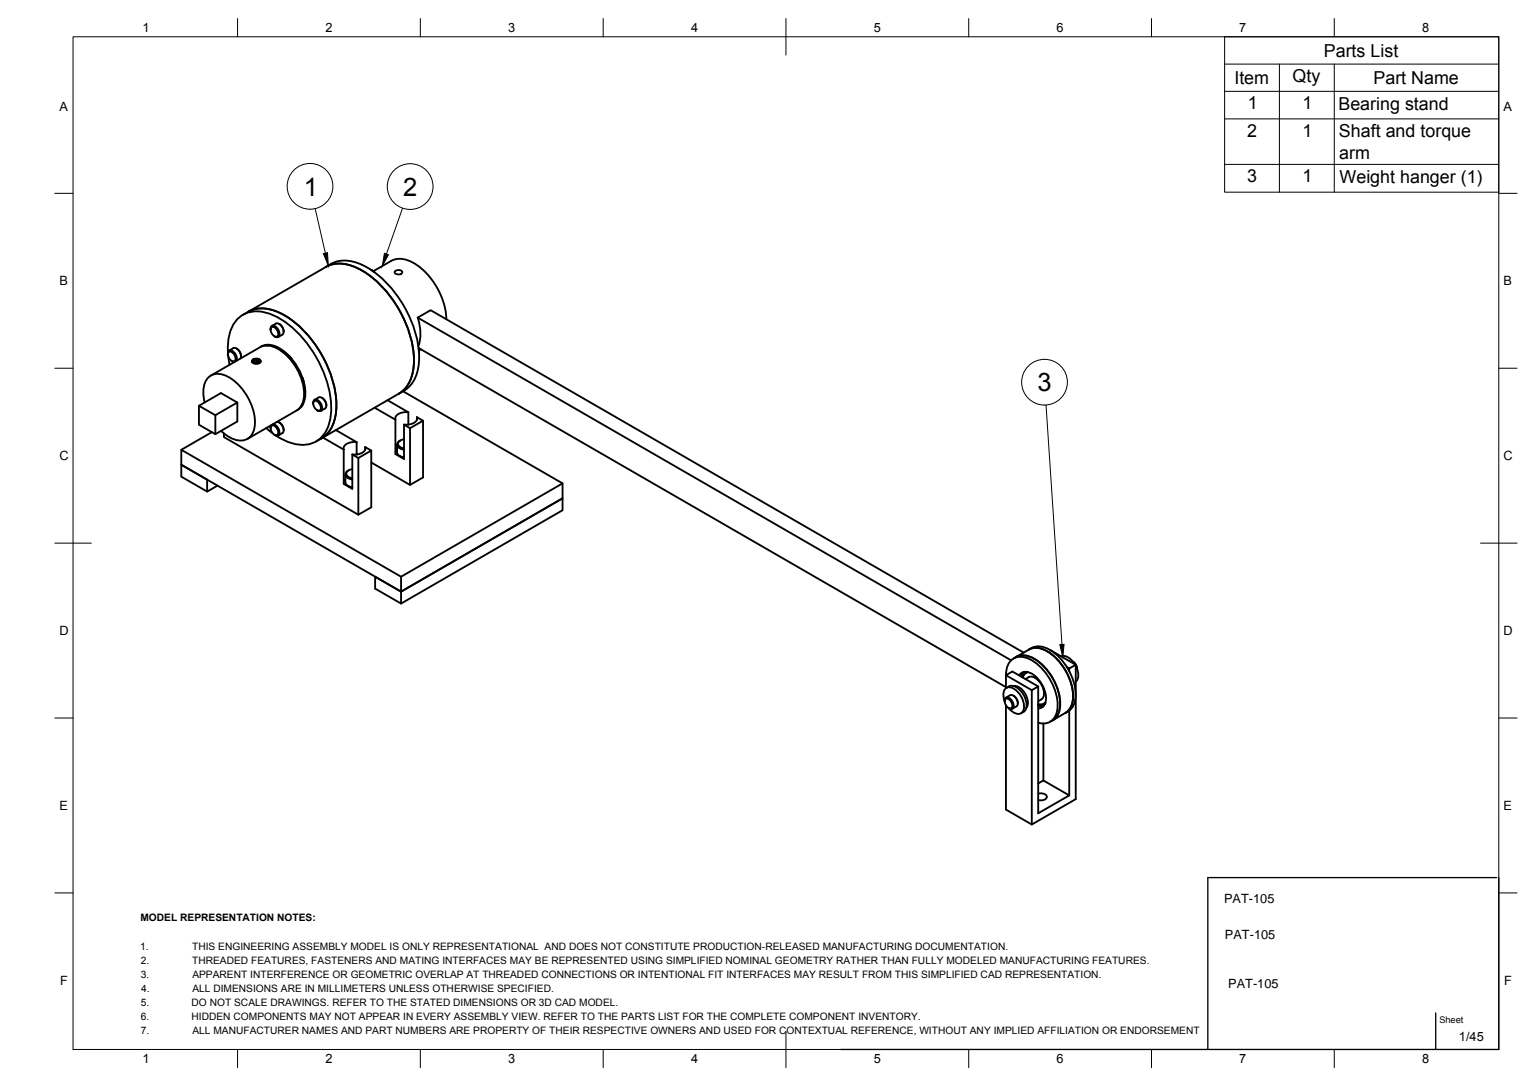
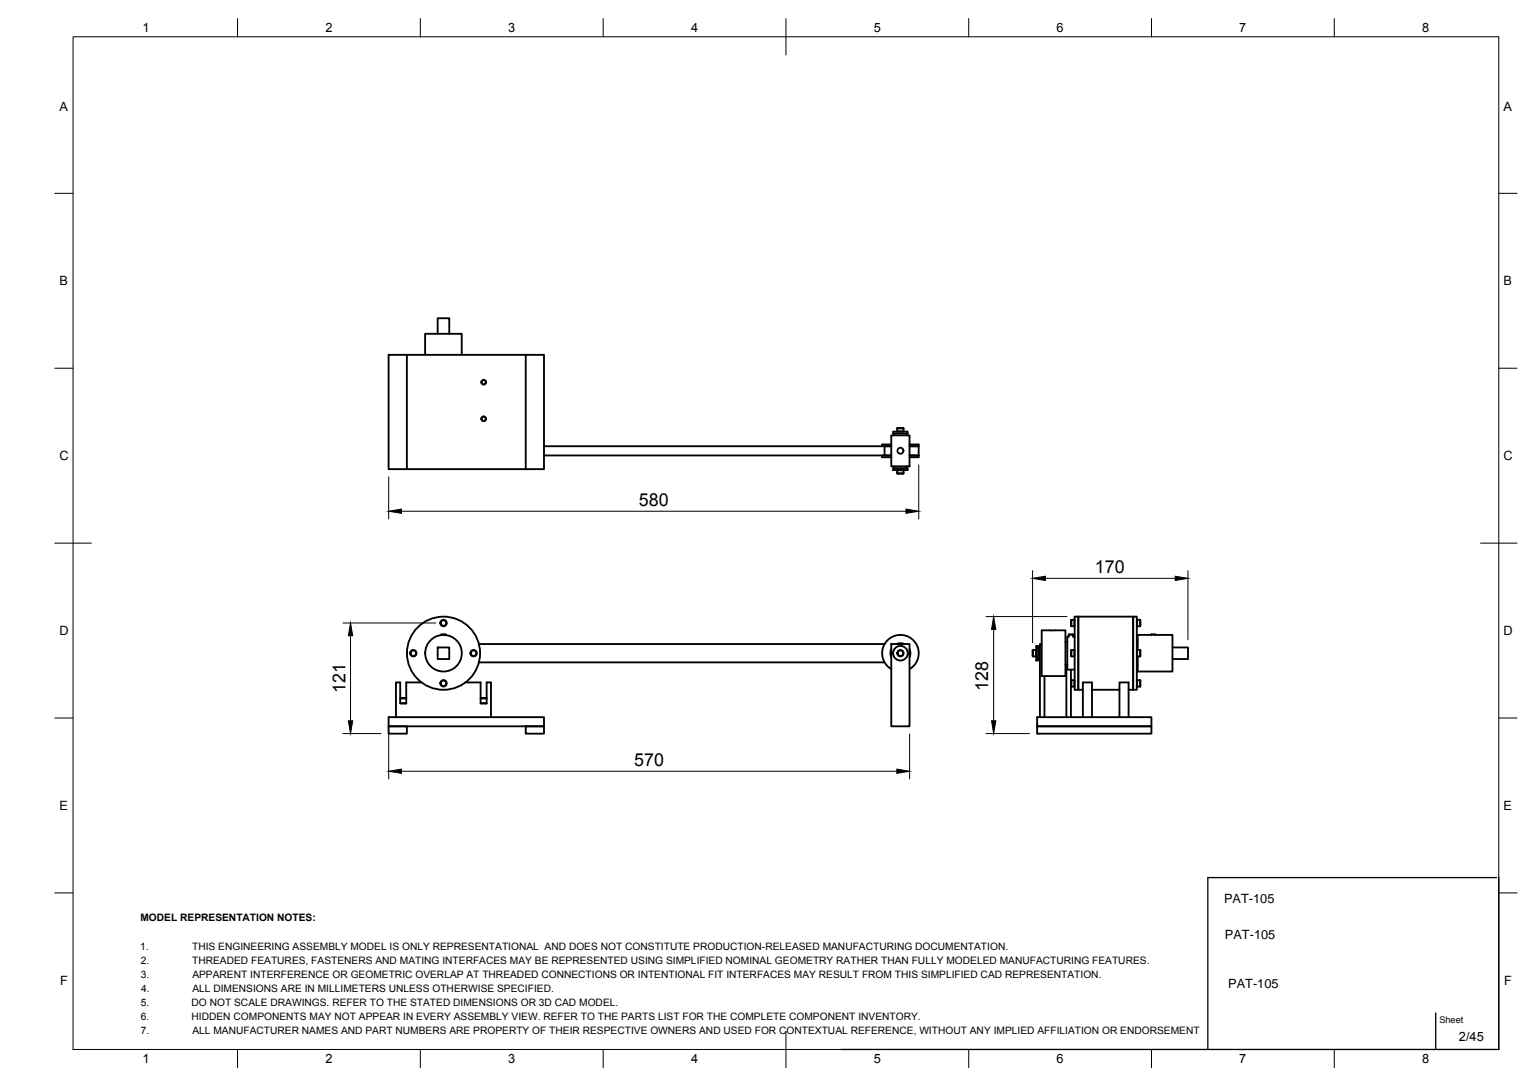
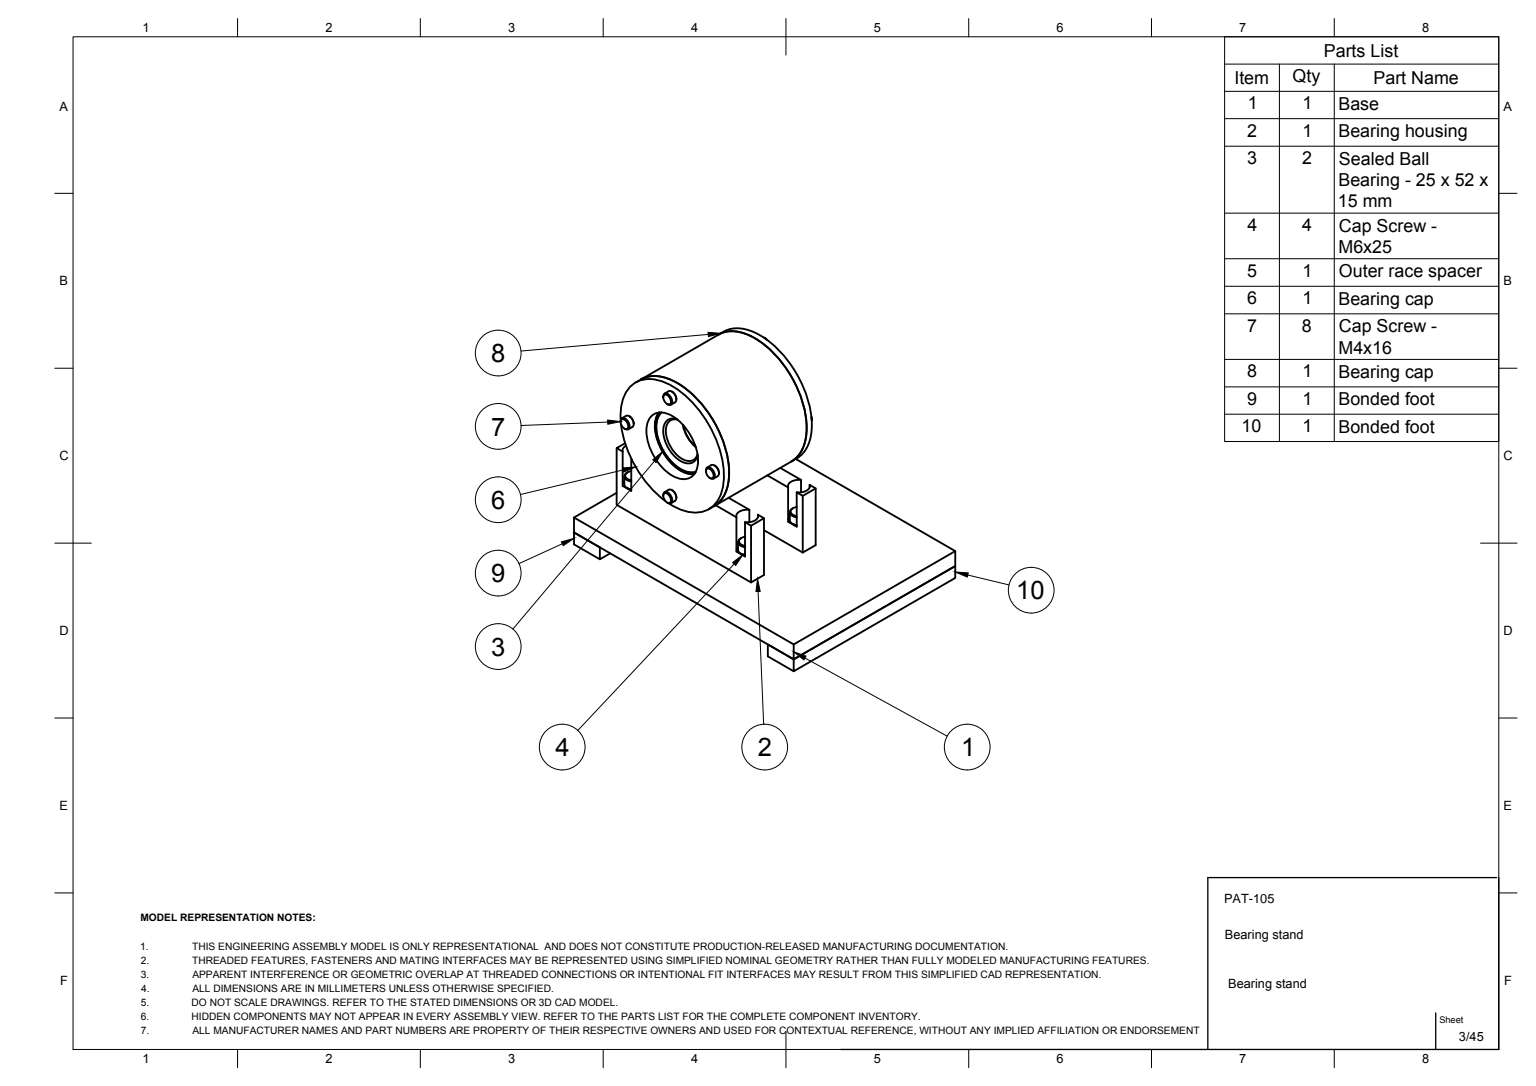
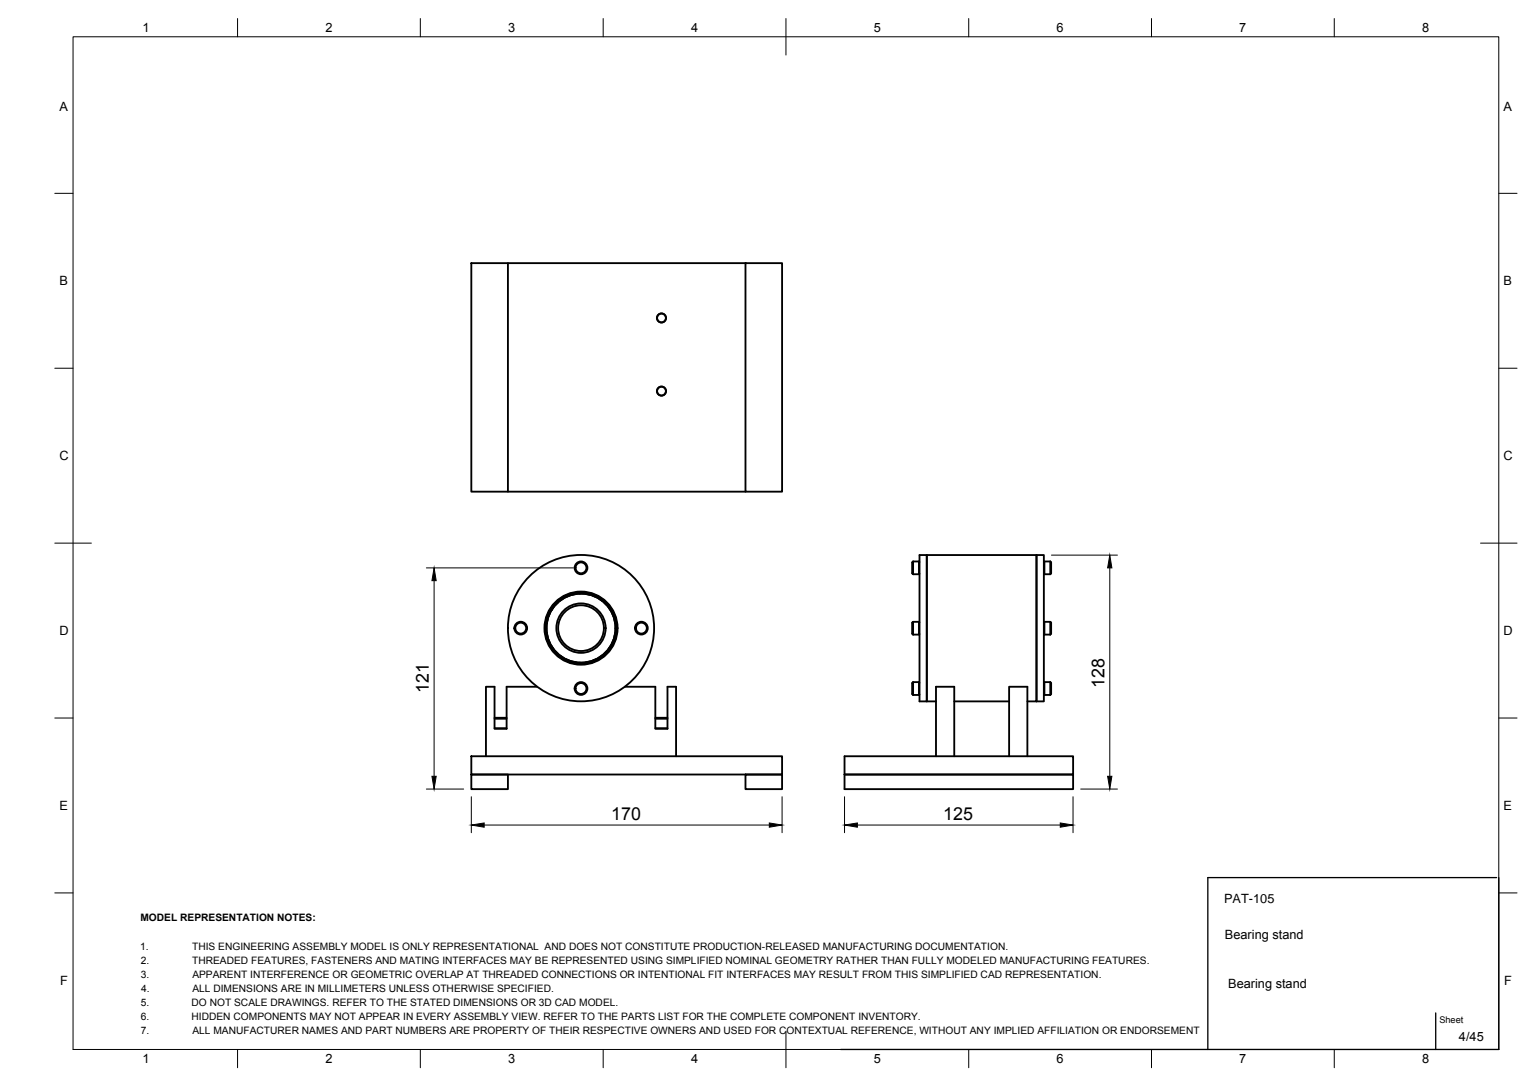
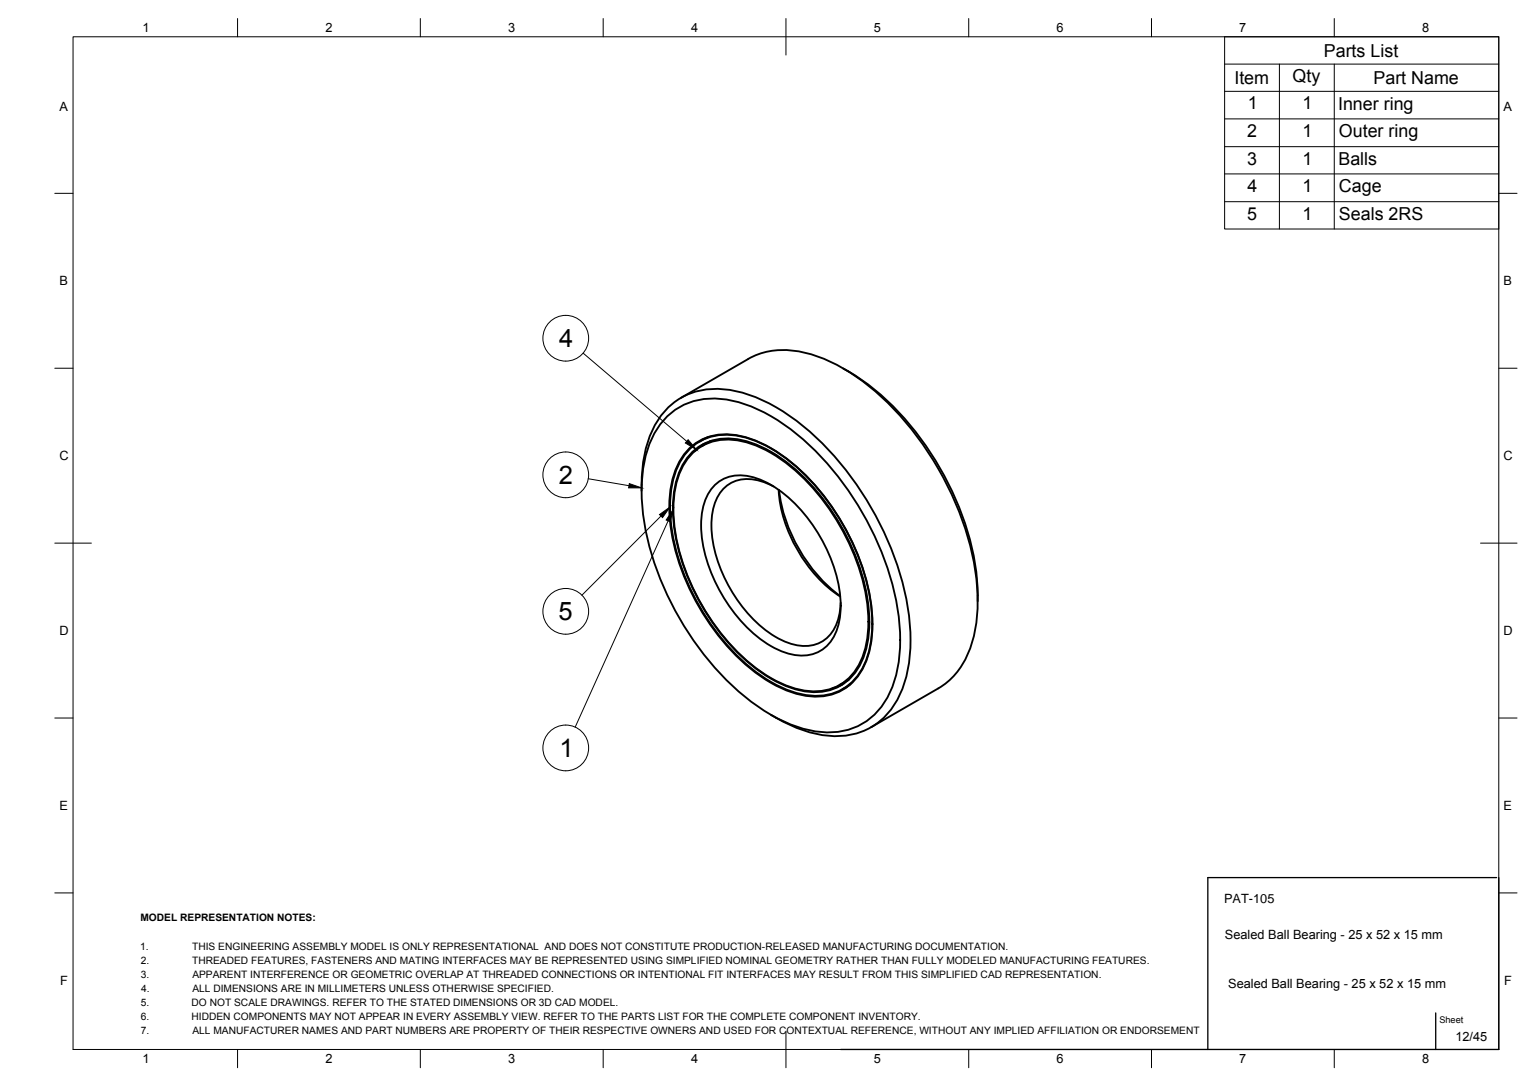
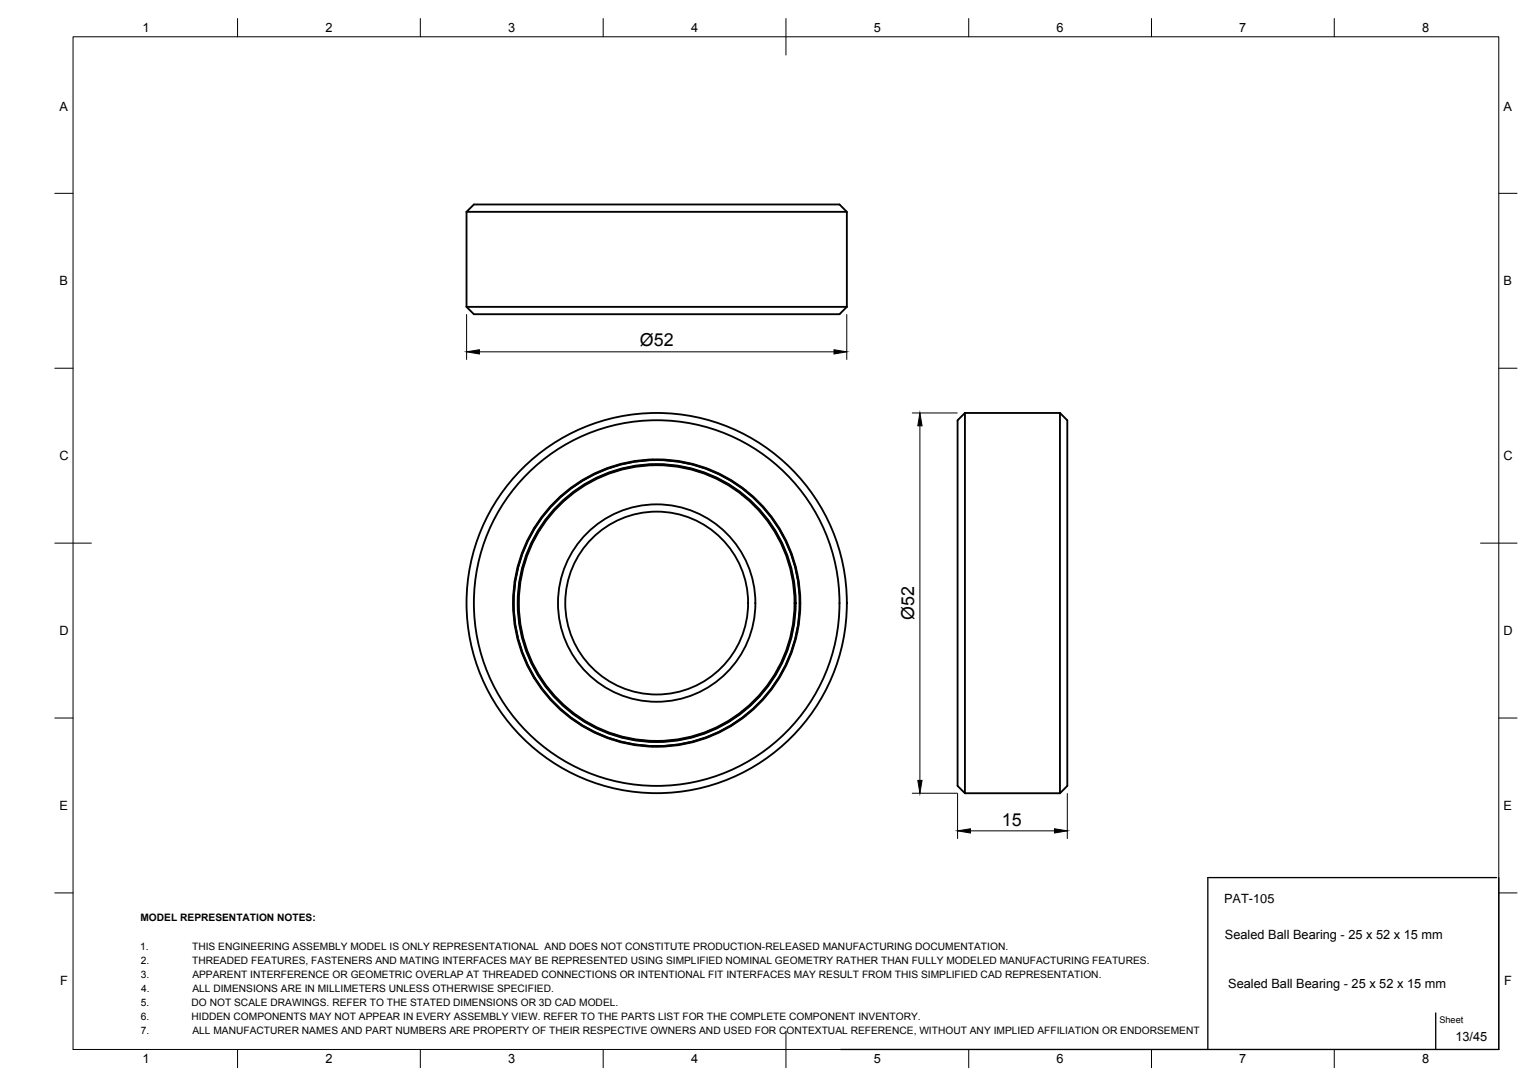
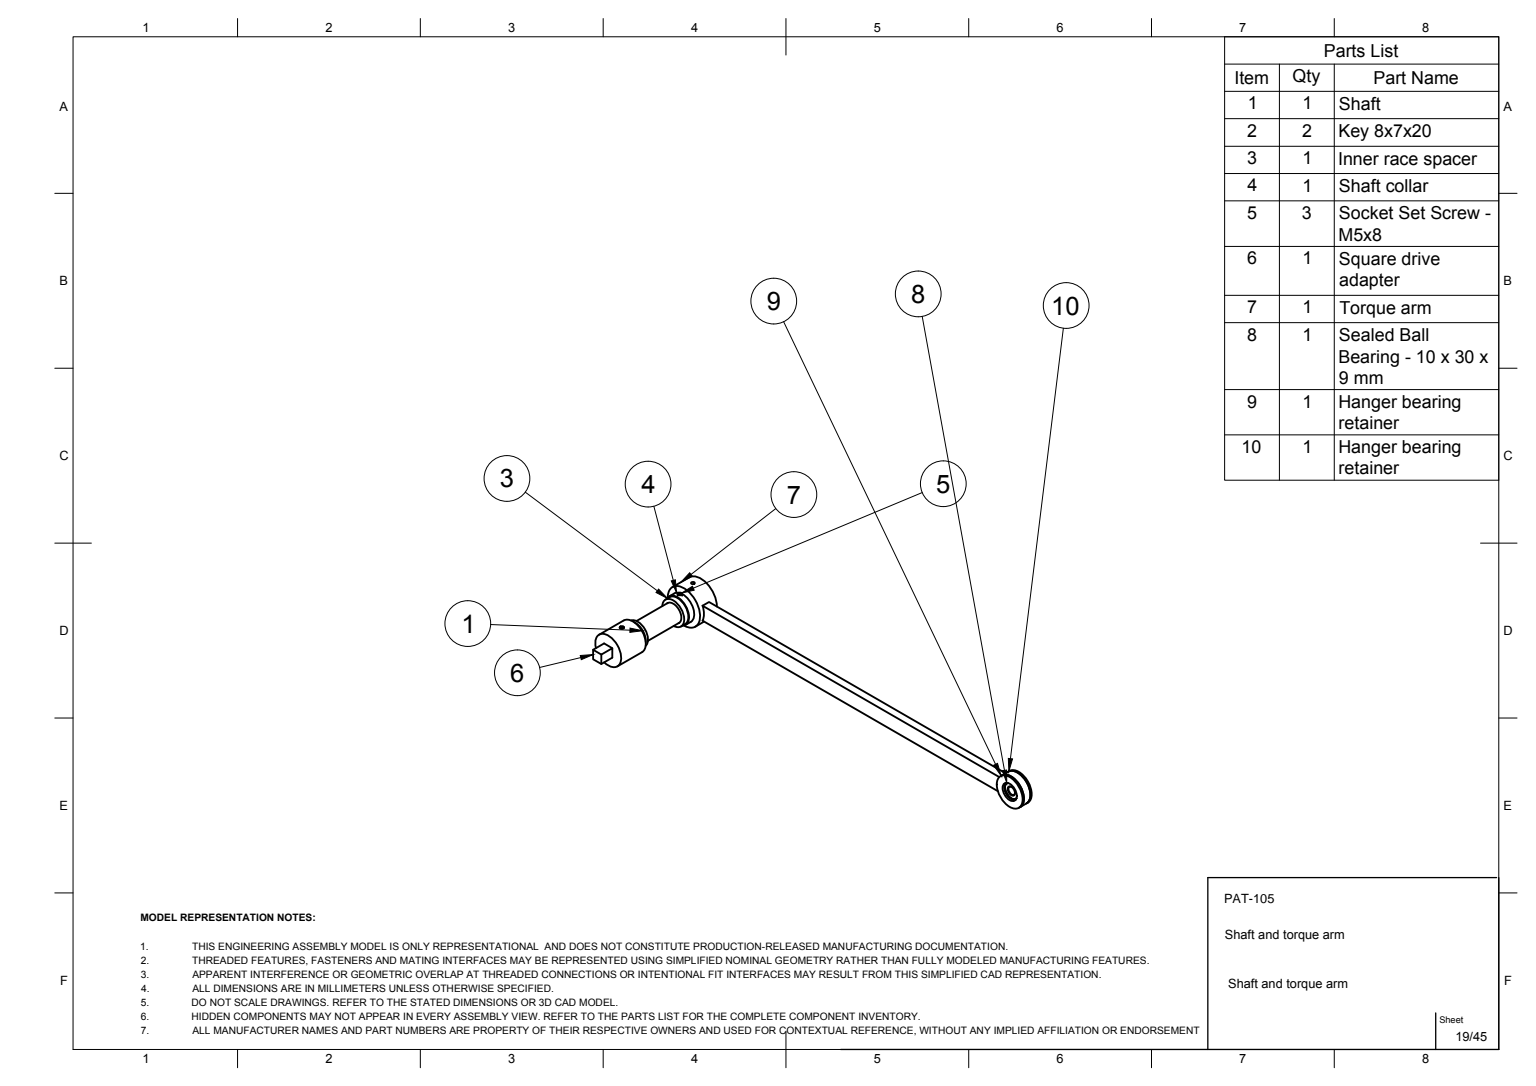
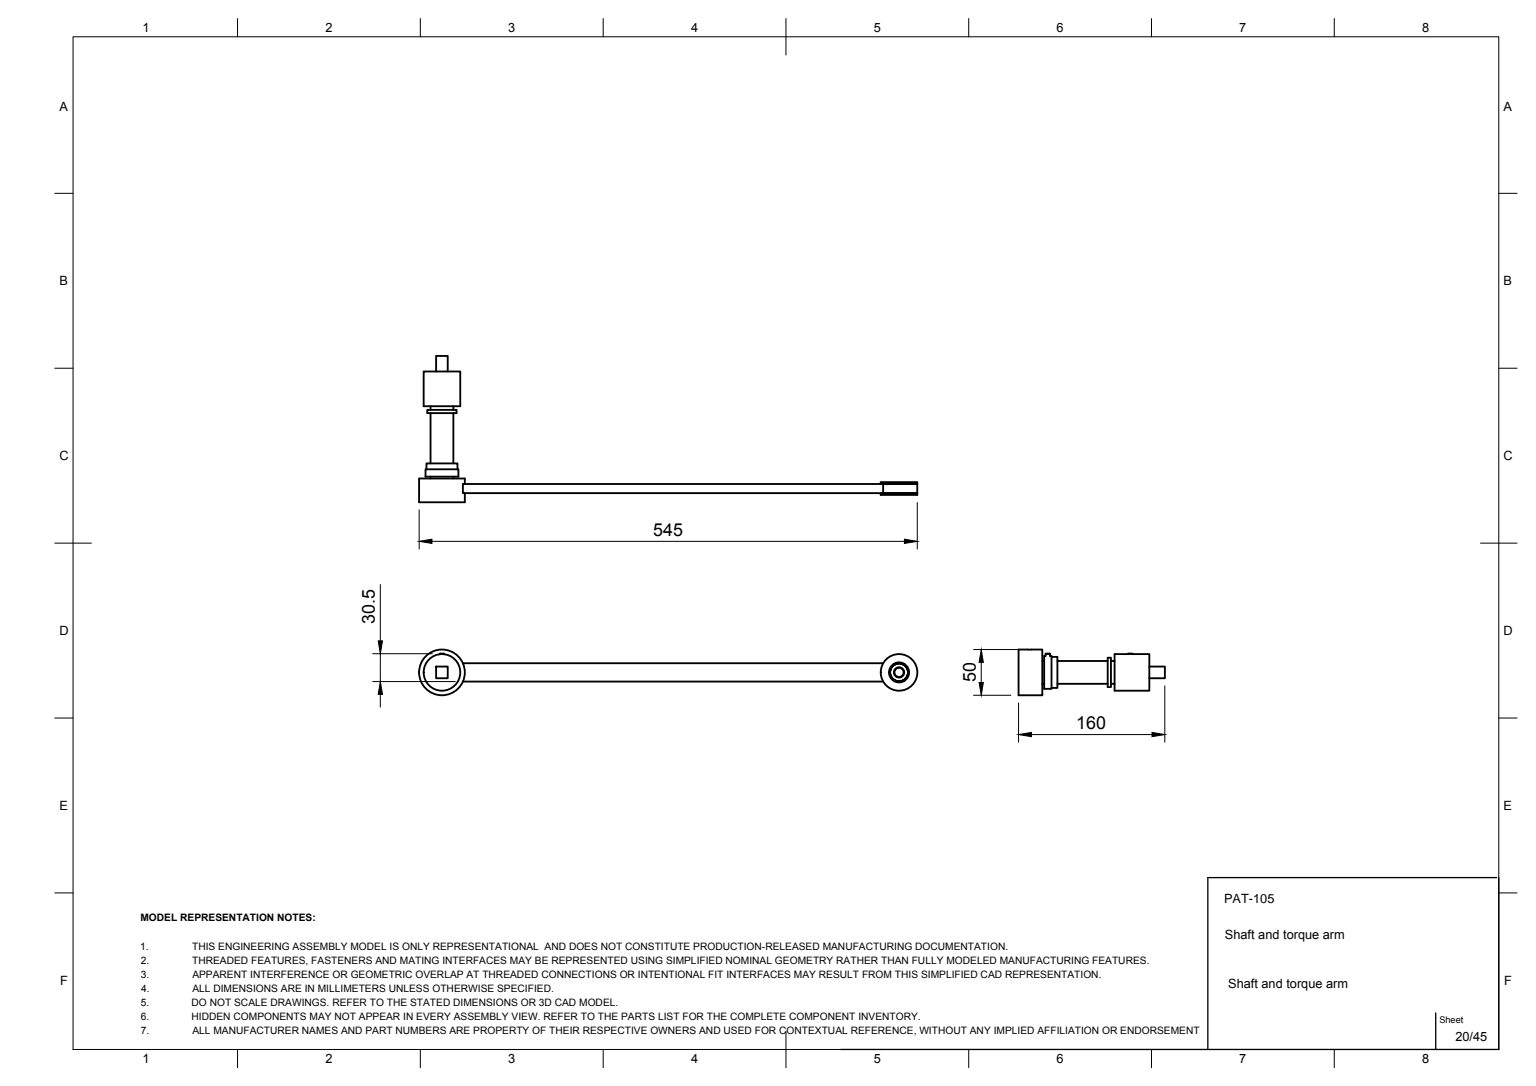
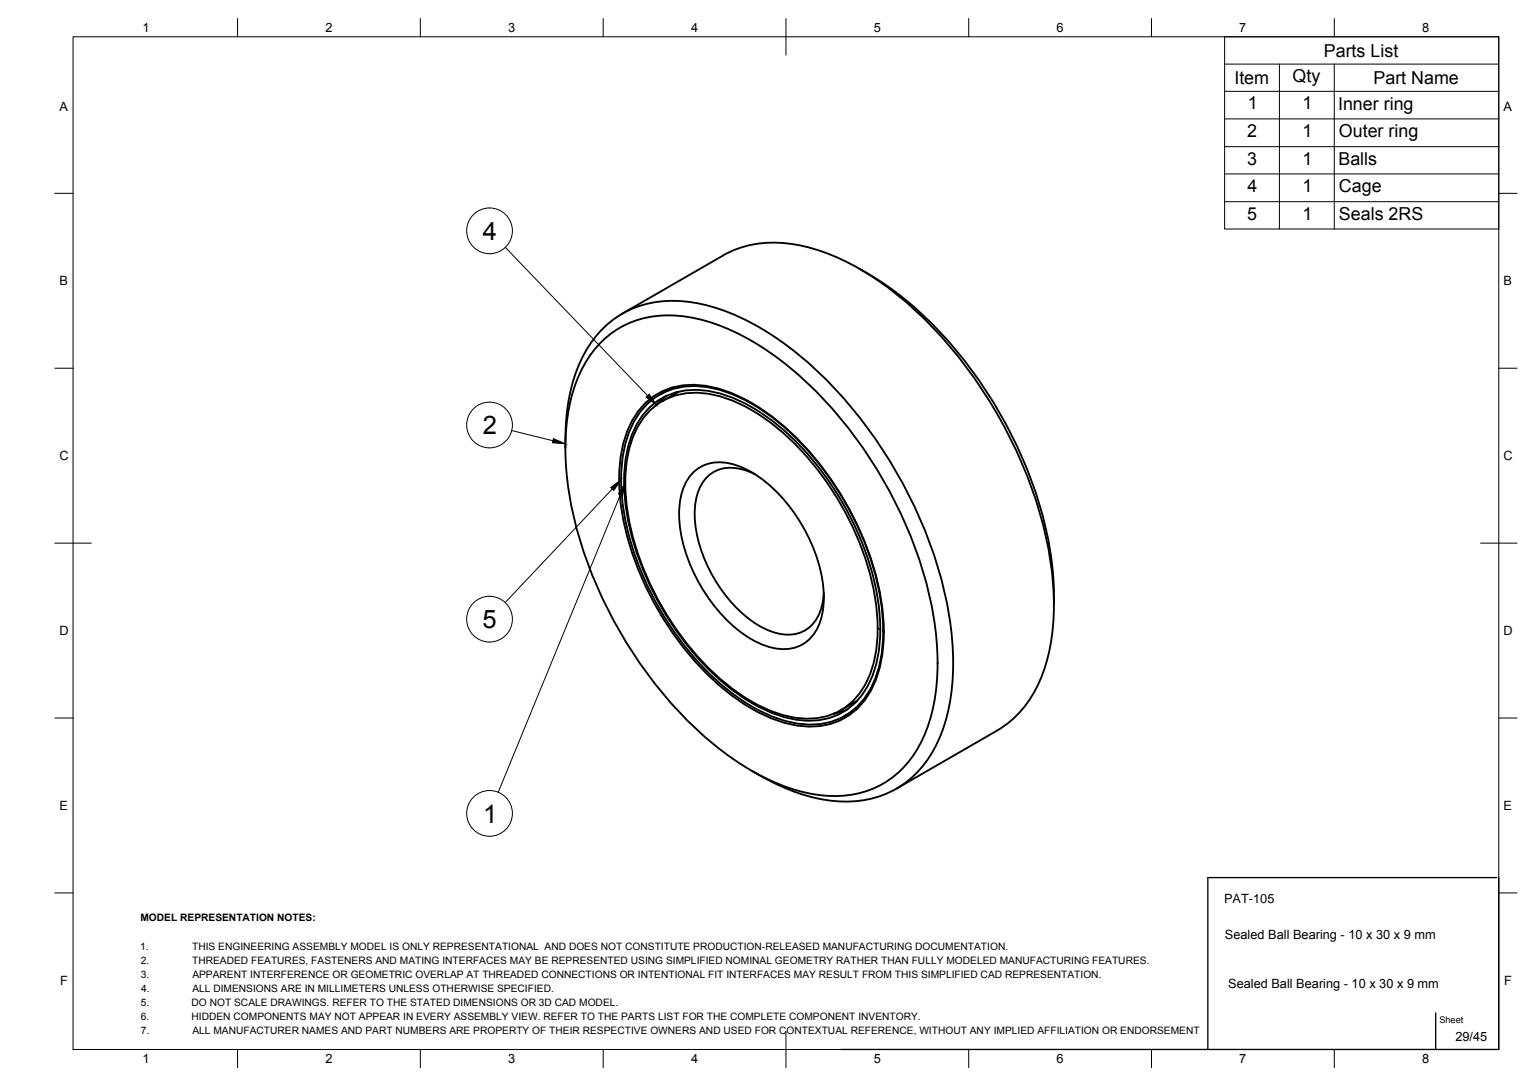
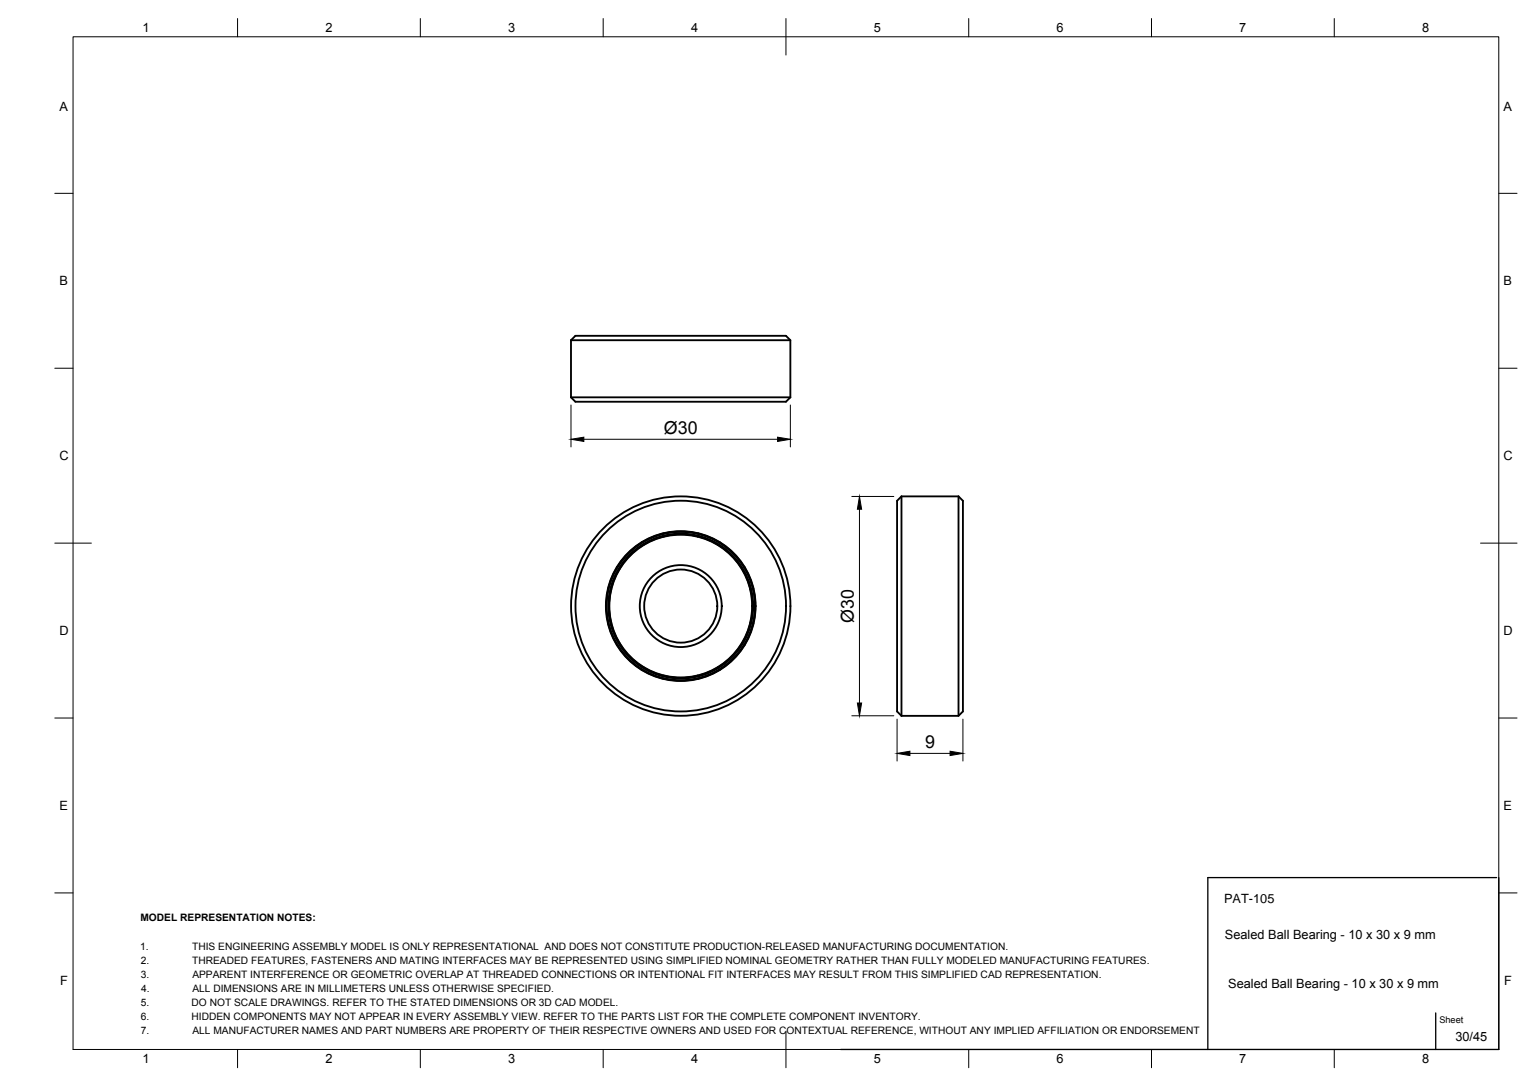
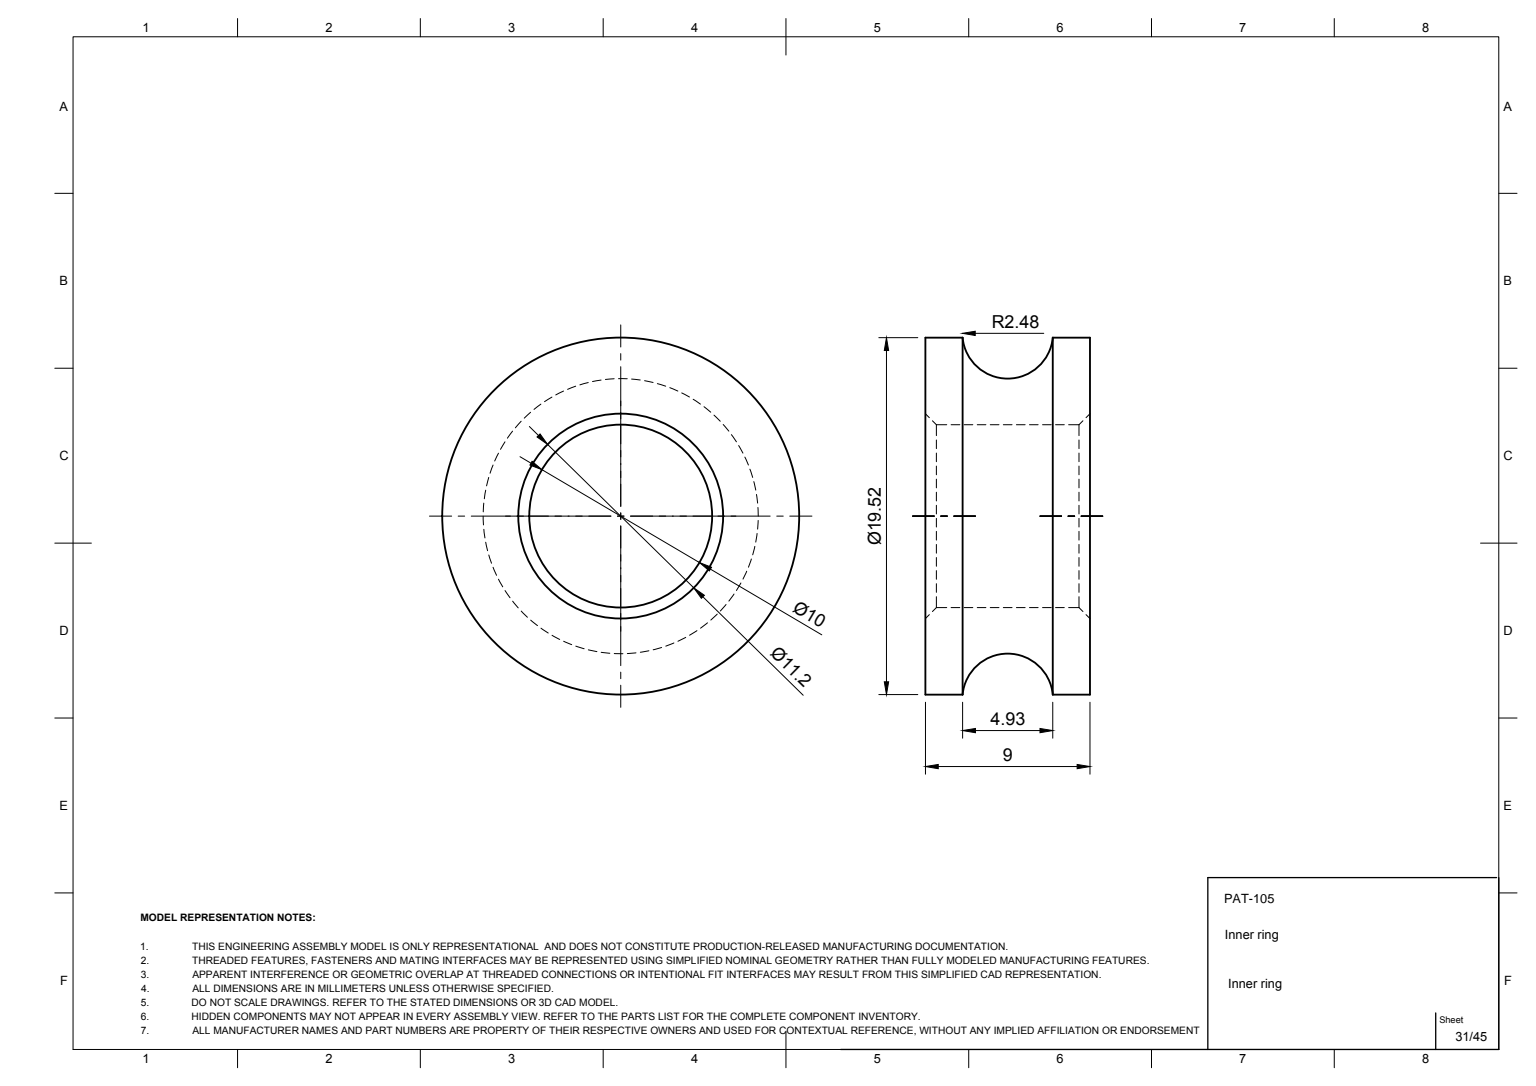
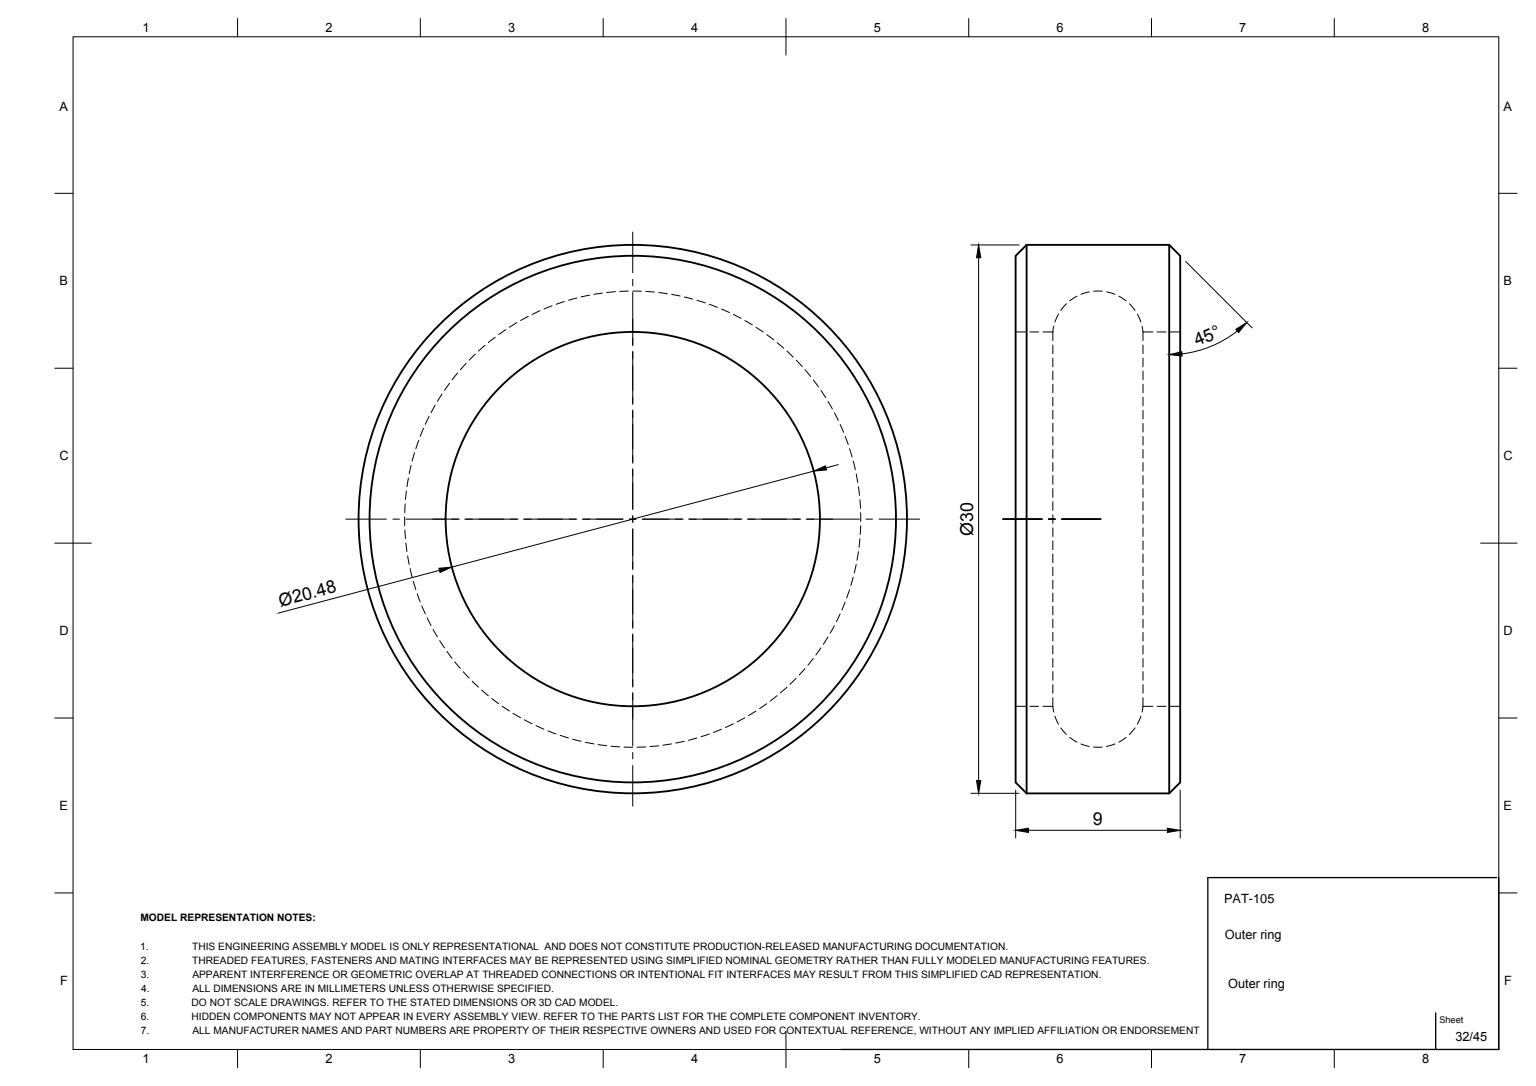
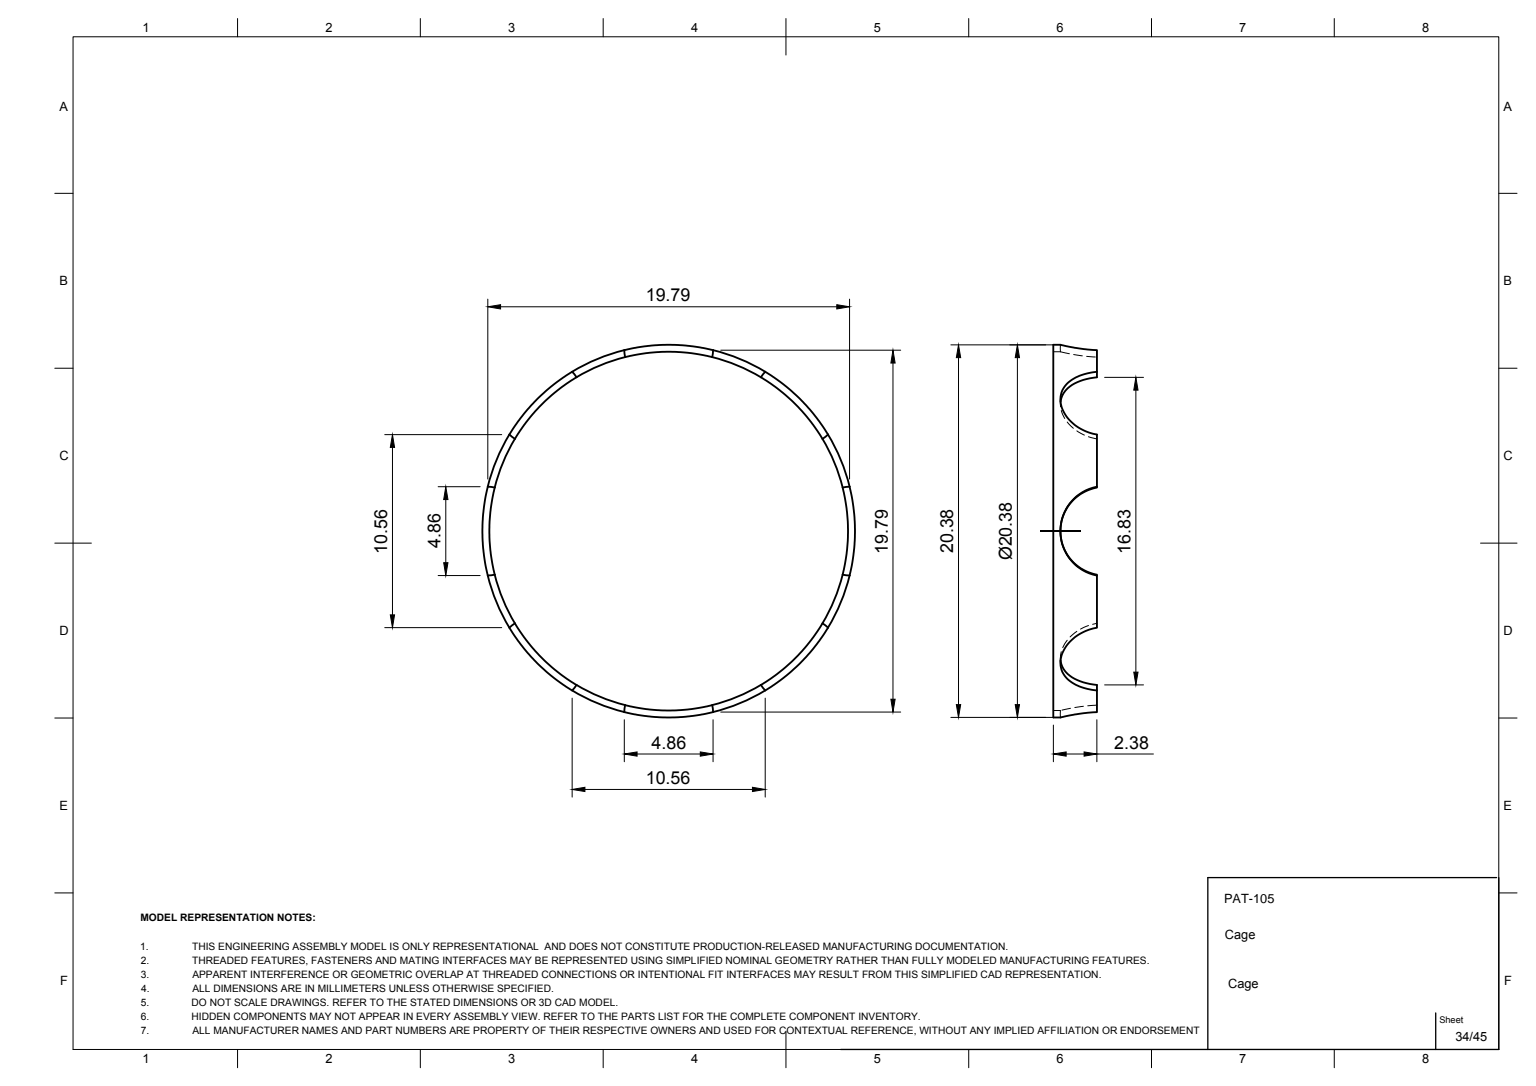
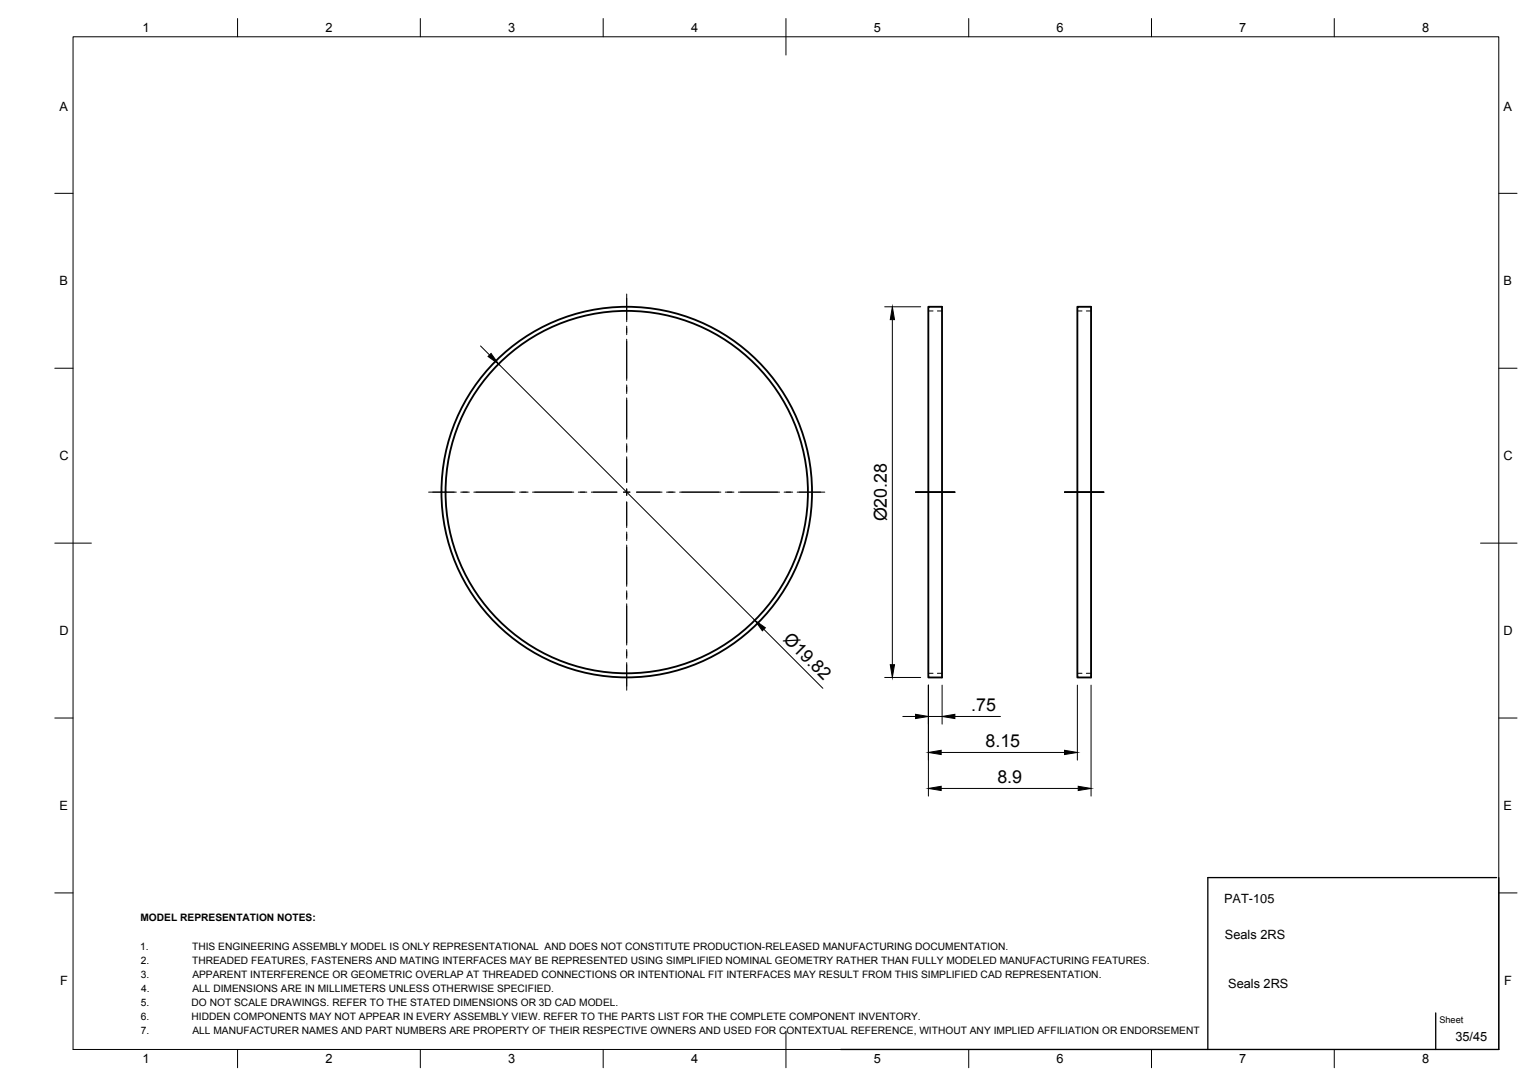
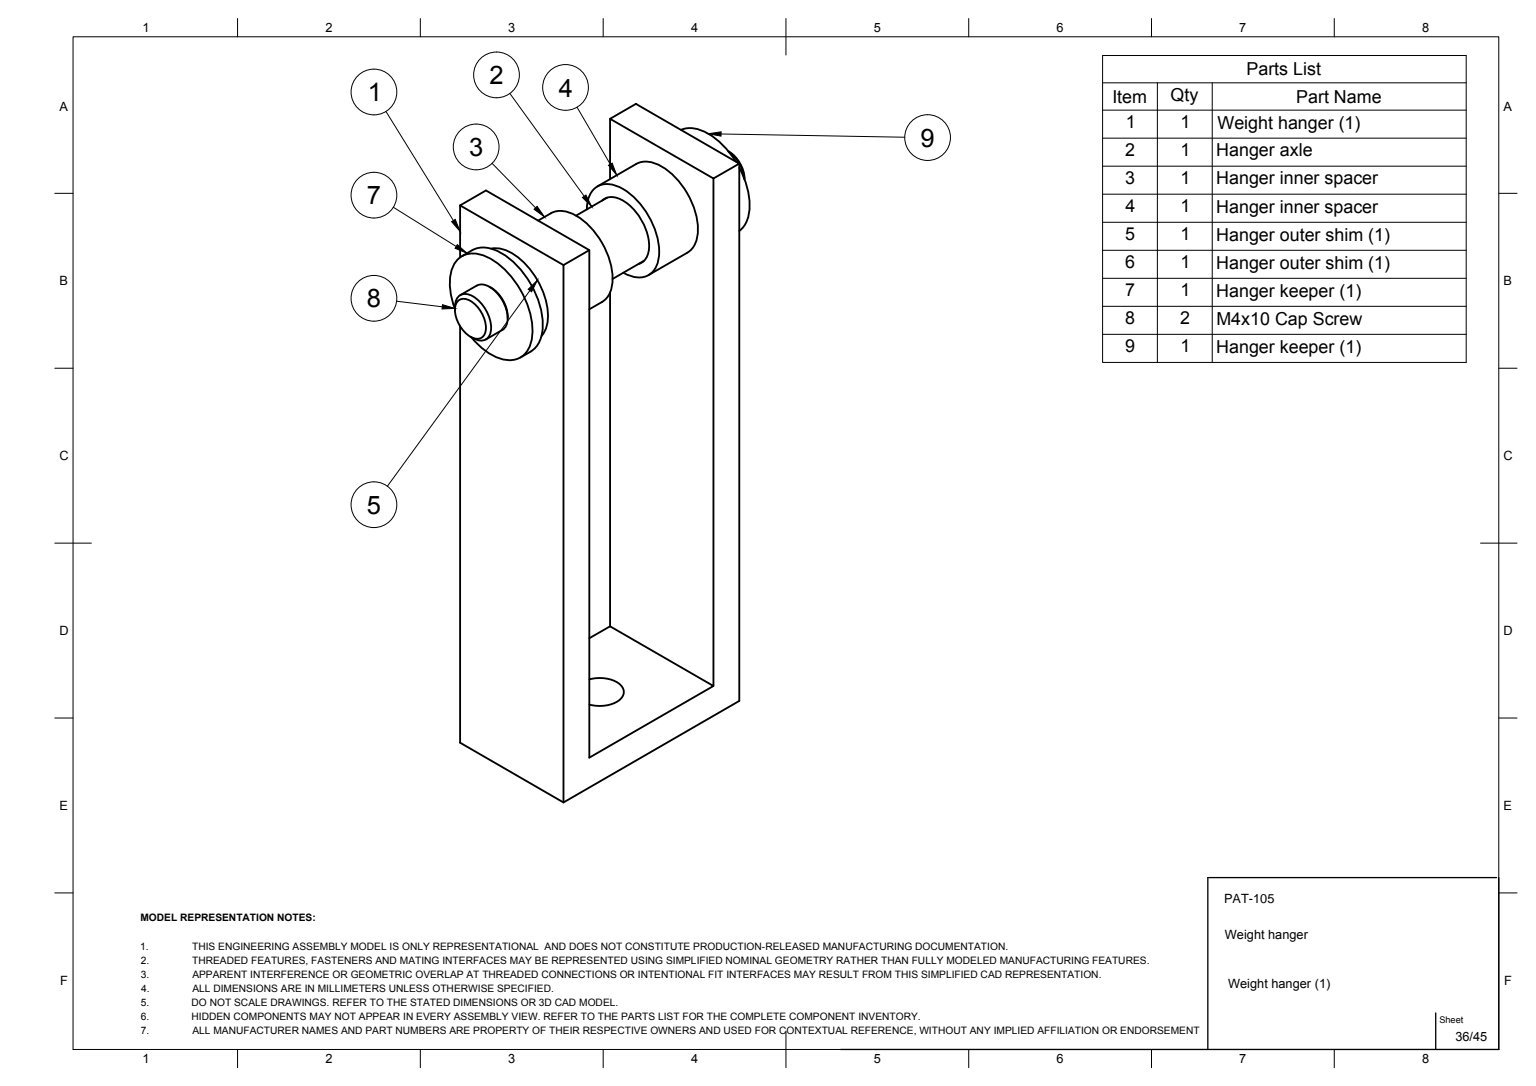
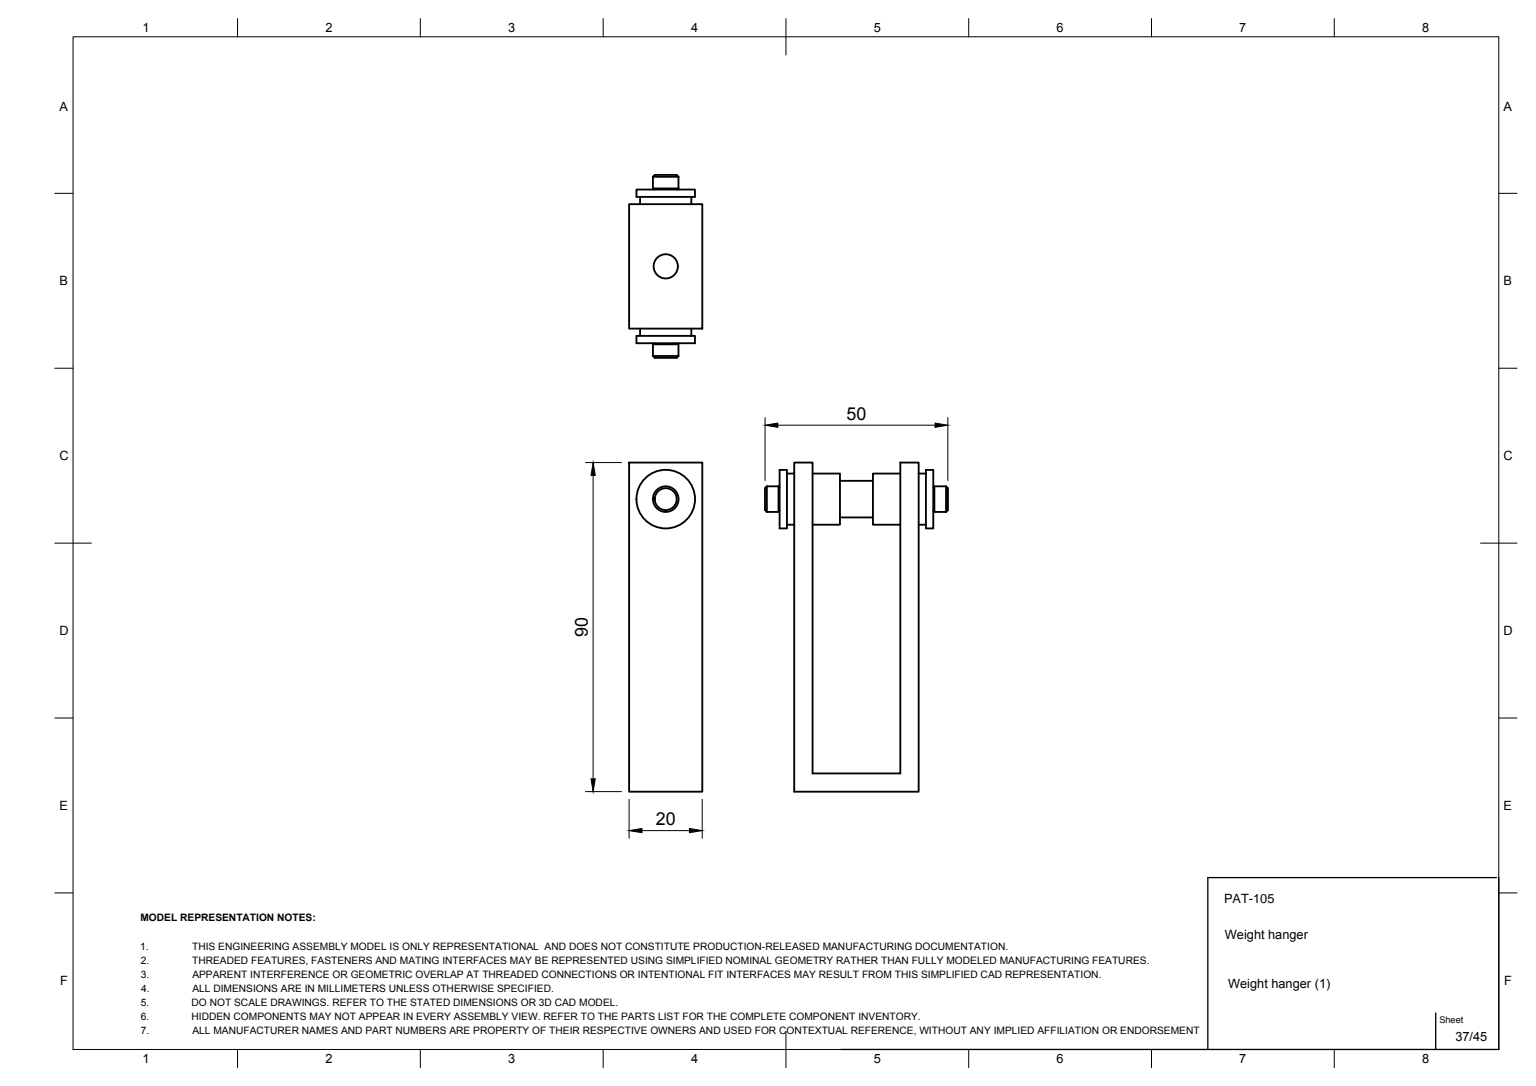
ISO-10303-21;
HEADER;
/* Generated by software containing ST-Developer
 * from STEP Tools, Inc. (www.steptools.com) 
 */

FILE_DESCRIPTION(
/* description */ ('Torque wrench calibration arm'),
/* implementation_level */ '2;1');

FILE_NAME(
/* name */ 'PAT-105',
/* time_stamp */ '2026-10-28T03:24:52-07:00',
/* author */ (''),
/* organization */ (''),
/* preprocessor_version */ 'ST-DEVELOPER v20.2',
/* originating_system */ 'Autodesk Translation Framework v15.17.0.0',
/* authorisation */ '');

FILE_SCHEMA (('AUTOMOTIVE_DESIGN { 1 0 10303 214 3 1 1 }'));
ENDSEC;

DATA;
#10=MECHANICAL_DESIGN_GEOMETRIC_PRESENTATION_REPRESENTATION('',(#426,#427,
#428,#429,#430,#431,#432,#433,#434,#435,#436,#437,#438,#439,#440,#441,#442,
#443,#444,#445,#446,#447,#448,#449,#450,#451,#452,#453,#454,#455,#456,#457,
#458,#459,#460,#461,#462,#463,#464,#465,#466,#467,#468,#469,#470,#471,#472,
#473,#474,#475,#476,#477,#478,#479),#12783);
#11=ORIENTED_CLOSED_SHELL('',*,#6517,.F.);
#12=ORIENTED_CLOSED_SHELL('',*,#6519,.F.);
#13=ORIENTED_CLOSED_SHELL('',*,#6550,.F.);
#14=BREP_WITH_VOIDS('Body1',#6516,(#11));
#15=BREP_WITH_VOIDS('Body1',#6518,(#12));
#16=BREP_WITH_VOIDS('Body1',#6551,(#13));
#17=ITEM_DEFINED_TRANSFORMATION($,$,#7158,#7296);
#18=ITEM_DEFINED_TRANSFORMATION($,$,#7178,#7297);
#19=ITEM_DEFINED_TRANSFORMATION($,$,#7198,#7298);
#20=ITEM_DEFINED_TRANSFORMATION($,$,#7217,#7299);
#21=ITEM_DEFINED_TRANSFORMATION($,$,#7279,#7300);
#22=ITEM_DEFINED_TRANSFORMATION($,$,#6962,#7353);
#23=ITEM_DEFINED_TRANSFORMATION($,$,#6981,#7354);
#24=ITEM_DEFINED_TRANSFORMATION($,$,#7084,#7355);
#25=ITEM_DEFINED_TRANSFORMATION($,$,#7093,#7356);
#26=ITEM_DEFINED_TRANSFORMATION($,$,#7118,#7357);
#27=ITEM_DEFINED_TRANSFORMATION($,$,#7143,#7358);
#28=ITEM_DEFINED_TRANSFORMATION($,$,#7150,#7359);
#29=ITEM_DEFINED_TRANSFORMATION($,$,#7157,#7360);
#30=ITEM_DEFINED_TRANSFORMATION($,$,#7301,#7361);
#31=ITEM_DEFINED_TRANSFORMATION($,$,#7301,#7362);
#32=ITEM_DEFINED_TRANSFORMATION($,$,#7157,#7363);
#33=ITEM_DEFINED_TRANSFORMATION($,$,#7301,#7364);
#34=ITEM_DEFINED_TRANSFORMATION($,$,#7301,#7365);
#35=ITEM_DEFINED_TRANSFORMATION($,$,#7327,#7366);
#36=ITEM_DEFINED_TRANSFORMATION($,$,#7327,#7367);
#37=ITEM_DEFINED_TRANSFORMATION($,$,#7327,#7368);
#38=ITEM_DEFINED_TRANSFORMATION($,$,#7327,#7369);
#39=ITEM_DEFINED_TRANSFORMATION($,$,#7327,#7370);
#40=ITEM_DEFINED_TRANSFORMATION($,$,#7327,#7371);
#41=ITEM_DEFINED_TRANSFORMATION($,$,#7327,#7372);
#42=ITEM_DEFINED_TRANSFORMATION($,$,#7327,#7373);
#43=ITEM_DEFINED_TRANSFORMATION($,$,#7538,#7666);
#44=ITEM_DEFINED_TRANSFORMATION($,$,#7558,#7667);
#45=ITEM_DEFINED_TRANSFORMATION($,$,#7578,#7668);
#46=ITEM_DEFINED_TRANSFORMATION($,$,#7595,#7669);
#47=ITEM_DEFINED_TRANSFORMATION($,$,#7649,#7670);
#48=ITEM_DEFINED_TRANSFORMATION($,$,#7375,#7671);
#49=ITEM_DEFINED_TRANSFORMATION($,$,#7403,#7672);
#50=ITEM_DEFINED_TRANSFORMATION($,$,#7412,#7673);
#51=ITEM_DEFINED_TRANSFORMATION($,$,#7427,#7674);
#52=ITEM_DEFINED_TRANSFORMATION($,$,#7453,#7675);
#53=ITEM_DEFINED_TRANSFORMATION($,$,#7483,#7676);
#54=ITEM_DEFINED_TRANSFORMATION($,$,#7496,#7677);
#55=ITEM_DEFINED_TRANSFORMATION($,$,#7509,#7678);
#56=ITEM_DEFINED_TRANSFORMATION($,$,#7509,#7679);
#57=ITEM_DEFINED_TRANSFORMATION($,$,#7520,#7680);
#58=ITEM_DEFINED_TRANSFORMATION($,$,#7520,#7681);
#59=ITEM_DEFINED_TRANSFORMATION($,$,#7520,#7682);
#60=ITEM_DEFINED_TRANSFORMATION($,$,#7537,#7683);
#61=ITEM_DEFINED_TRANSFORMATION($,$,#7685,#7797);
#62=ITEM_DEFINED_TRANSFORMATION($,$,#7705,#7798);
#63=ITEM_DEFINED_TRANSFORMATION($,$,#7719,#7799);
#64=ITEM_DEFINED_TRANSFORMATION($,$,#7728,#7800);
#65=ITEM_DEFINED_TRANSFORMATION($,$,#7737,#7801);
#66=ITEM_DEFINED_TRANSFORMATION($,$,#7746,#7802);
#67=ITEM_DEFINED_TRANSFORMATION($,$,#7755,#7803);
#68=ITEM_DEFINED_TRANSFORMATION($,$,#7764,#7804);
#69=ITEM_DEFINED_TRANSFORMATION($,$,#7773,#7805);
#70=ITEM_DEFINED_TRANSFORMATION($,$,#7773,#7806);
#71=ITEM_DEFINED_TRANSFORMATION($,$,#6961,#7807);
#72=ITEM_DEFINED_TRANSFORMATION($,$,#7374,#7808);
#73=ITEM_DEFINED_TRANSFORMATION($,$,#7684,#7809);
#74=(
REPRESENTATION_RELATIONSHIP($,$,#12941,#12940)
REPRESENTATION_RELATIONSHIP_WITH_TRANSFORMATION(#17)
SHAPE_REPRESENTATION_RELATIONSHIP()
);
#75=(
REPRESENTATION_RELATIONSHIP($,$,#12942,#12940)
REPRESENTATION_RELATIONSHIP_WITH_TRANSFORMATION(#18)
SHAPE_REPRESENTATION_RELATIONSHIP()
);
#76=(
REPRESENTATION_RELATIONSHIP($,$,#12943,#12940)
REPRESENTATION_RELATIONSHIP_WITH_TRANSFORMATION(#19)
SHAPE_REPRESENTATION_RELATIONSHIP()
);
#77=(
REPRESENTATION_RELATIONSHIP($,$,#12944,#12940)
REPRESENTATION_RELATIONSHIP_WITH_TRANSFORMATION(#20)
SHAPE_REPRESENTATION_RELATIONSHIP()
);
#78=(
REPRESENTATION_RELATIONSHIP($,$,#12945,#12940)
REPRESENTATION_RELATIONSHIP_WITH_TRANSFORMATION(#21)
SHAPE_REPRESENTATION_RELATIONSHIP()
);
#79=(
REPRESENTATION_RELATIONSHIP($,$,#12933,#12932)
REPRESENTATION_RELATIONSHIP_WITH_TRANSFORMATION(#22)
SHAPE_REPRESENTATION_RELATIONSHIP()
);
#80=(
REPRESENTATION_RELATIONSHIP($,$,#12934,#12932)
REPRESENTATION_RELATIONSHIP_WITH_TRANSFORMATION(#23)
SHAPE_REPRESENTATION_RELATIONSHIP()
);
#81=(
REPRESENTATION_RELATIONSHIP($,$,#12935,#12932)
REPRESENTATION_RELATIONSHIP_WITH_TRANSFORMATION(#24)
SHAPE_REPRESENTATION_RELATIONSHIP()
);
#82=(
REPRESENTATION_RELATIONSHIP($,$,#12936,#12932)
REPRESENTATION_RELATIONSHIP_WITH_TRANSFORMATION(#25)
SHAPE_REPRESENTATION_RELATIONSHIP()
);
#83=(
REPRESENTATION_RELATIONSHIP($,$,#12937,#12932)
REPRESENTATION_RELATIONSHIP_WITH_TRANSFORMATION(#26)
SHAPE_REPRESENTATION_RELATIONSHIP()
);
#84=(
REPRESENTATION_RELATIONSHIP($,$,#12938,#12932)
REPRESENTATION_RELATIONSHIP_WITH_TRANSFORMATION(#27)
SHAPE_REPRESENTATION_RELATIONSHIP()
);
#85=(
REPRESENTATION_RELATIONSHIP($,$,#12939,#12932)
REPRESENTATION_RELATIONSHIP_WITH_TRANSFORMATION(#28)
SHAPE_REPRESENTATION_RELATIONSHIP()
);
#86=(
REPRESENTATION_RELATIONSHIP($,$,#12940,#12932)
REPRESENTATION_RELATIONSHIP_WITH_TRANSFORMATION(#29)
SHAPE_REPRESENTATION_RELATIONSHIP()
);
#87=(
REPRESENTATION_RELATIONSHIP($,$,#12946,#12932)
REPRESENTATION_RELATIONSHIP_WITH_TRANSFORMATION(#30)
SHAPE_REPRESENTATION_RELATIONSHIP()
);
#88=(
REPRESENTATION_RELATIONSHIP($,$,#12946,#12932)
REPRESENTATION_RELATIONSHIP_WITH_TRANSFORMATION(#31)
SHAPE_REPRESENTATION_RELATIONSHIP()
);
#89=(
REPRESENTATION_RELATIONSHIP($,$,#12940,#12932)
REPRESENTATION_RELATIONSHIP_WITH_TRANSFORMATION(#32)
SHAPE_REPRESENTATION_RELATIONSHIP()
);
#90=(
REPRESENTATION_RELATIONSHIP($,$,#12946,#12932)
REPRESENTATION_RELATIONSHIP_WITH_TRANSFORMATION(#33)
SHAPE_REPRESENTATION_RELATIONSHIP()
);
#91=(
REPRESENTATION_RELATIONSHIP($,$,#12946,#12932)
REPRESENTATION_RELATIONSHIP_WITH_TRANSFORMATION(#34)
SHAPE_REPRESENTATION_RELATIONSHIP()
);
#92=(
REPRESENTATION_RELATIONSHIP($,$,#12947,#12932)
REPRESENTATION_RELATIONSHIP_WITH_TRANSFORMATION(#35)
SHAPE_REPRESENTATION_RELATIONSHIP()
);
#93=(
REPRESENTATION_RELATIONSHIP($,$,#12947,#12932)
REPRESENTATION_RELATIONSHIP_WITH_TRANSFORMATION(#36)
SHAPE_REPRESENTATION_RELATIONSHIP()
);
#94=(
REPRESENTATION_RELATIONSHIP($,$,#12947,#12932)
REPRESENTATION_RELATIONSHIP_WITH_TRANSFORMATION(#37)
SHAPE_REPRESENTATION_RELATIONSHIP()
);
#95=(
REPRESENTATION_RELATIONSHIP($,$,#12947,#12932)
REPRESENTATION_RELATIONSHIP_WITH_TRANSFORMATION(#38)
SHAPE_REPRESENTATION_RELATIONSHIP()
);
#96=(
REPRESENTATION_RELATIONSHIP($,$,#12947,#12932)
REPRESENTATION_RELATIONSHIP_WITH_TRANSFORMATION(#39)
SHAPE_REPRESENTATION_RELATIONSHIP()
);
#97=(
REPRESENTATION_RELATIONSHIP($,$,#12947,#12932)
REPRESENTATION_RELATIONSHIP_WITH_TRANSFORMATION(#40)
SHAPE_REPRESENTATION_RELATIONSHIP()
);
#98=(
REPRESENTATION_RELATIONSHIP($,$,#12947,#12932)
REPRESENTATION_RELATIONSHIP_WITH_TRANSFORMATION(#41)
SHAPE_REPRESENTATION_RELATIONSHIP()
);
#99=(
REPRESENTATION_RELATIONSHIP($,$,#12947,#12932)
REPRESENTATION_RELATIONSHIP_WITH_TRANSFORMATION(#42)
SHAPE_REPRESENTATION_RELATIONSHIP()
);
#100=(
REPRESENTATION_RELATIONSHIP($,$,#12959,#12958)
REPRESENTATION_RELATIONSHIP_WITH_TRANSFORMATION(#43)
SHAPE_REPRESENTATION_RELATIONSHIP()
);
#101=(
REPRESENTATION_RELATIONSHIP($,$,#12960,#12958)
REPRESENTATION_RELATIONSHIP_WITH_TRANSFORMATION(#44)
SHAPE_REPRESENTATION_RELATIONSHIP()
);
#102=(
REPRESENTATION_RELATIONSHIP($,$,#12961,#12958)
REPRESENTATION_RELATIONSHIP_WITH_TRANSFORMATION(#45)
SHAPE_REPRESENTATION_RELATIONSHIP()
);
#103=(
REPRESENTATION_RELATIONSHIP($,$,#12962,#12958)
REPRESENTATION_RELATIONSHIP_WITH_TRANSFORMATION(#46)
SHAPE_REPRESENTATION_RELATIONSHIP()
);
#104=(
REPRESENTATION_RELATIONSHIP($,$,#12963,#12958)
REPRESENTATION_RELATIONSHIP_WITH_TRANSFORMATION(#47)
SHAPE_REPRESENTATION_RELATIONSHIP()
);
#105=(
REPRESENTATION_RELATIONSHIP($,$,#12949,#12948)
REPRESENTATION_RELATIONSHIP_WITH_TRANSFORMATION(#48)
SHAPE_REPRESENTATION_RELATIONSHIP()
);
#106=(
REPRESENTATION_RELATIONSHIP($,$,#12950,#12948)
REPRESENTATION_RELATIONSHIP_WITH_TRANSFORMATION(#49)
SHAPE_REPRESENTATION_RELATIONSHIP()
);
#107=(
REPRESENTATION_RELATIONSHIP($,$,#12951,#12948)
REPRESENTATION_RELATIONSHIP_WITH_TRANSFORMATION(#50)
SHAPE_REPRESENTATION_RELATIONSHIP()
);
#108=(
REPRESENTATION_RELATIONSHIP($,$,#12952,#12948)
REPRESENTATION_RELATIONSHIP_WITH_TRANSFORMATION(#51)
SHAPE_REPRESENTATION_RELATIONSHIP()
);
#109=(
REPRESENTATION_RELATIONSHIP($,$,#12953,#12948)
REPRESENTATION_RELATIONSHIP_WITH_TRANSFORMATION(#52)
SHAPE_REPRESENTATION_RELATIONSHIP()
);
#110=(
REPRESENTATION_RELATIONSHIP($,$,#12954,#12948)
REPRESENTATION_RELATIONSHIP_WITH_TRANSFORMATION(#53)
SHAPE_REPRESENTATION_RELATIONSHIP()
);
#111=(
REPRESENTATION_RELATIONSHIP($,$,#12955,#12948)
REPRESENTATION_RELATIONSHIP_WITH_TRANSFORMATION(#54)
SHAPE_REPRESENTATION_RELATIONSHIP()
);
#112=(
REPRESENTATION_RELATIONSHIP($,$,#12956,#12948)
REPRESENTATION_RELATIONSHIP_WITH_TRANSFORMATION(#55)
SHAPE_REPRESENTATION_RELATIONSHIP()
);
#113=(
REPRESENTATION_RELATIONSHIP($,$,#12956,#12948)
REPRESENTATION_RELATIONSHIP_WITH_TRANSFORMATION(#56)
SHAPE_REPRESENTATION_RELATIONSHIP()
);
#114=(
REPRESENTATION_RELATIONSHIP($,$,#12957,#12948)
REPRESENTATION_RELATIONSHIP_WITH_TRANSFORMATION(#57)
SHAPE_REPRESENTATION_RELATIONSHIP()
);
#115=(
REPRESENTATION_RELATIONSHIP($,$,#12957,#12948)
REPRESENTATION_RELATIONSHIP_WITH_TRANSFORMATION(#58)
SHAPE_REPRESENTATION_RELATIONSHIP()
);
#116=(
REPRESENTATION_RELATIONSHIP($,$,#12957,#12948)
REPRESENTATION_RELATIONSHIP_WITH_TRANSFORMATION(#59)
SHAPE_REPRESENTATION_RELATIONSHIP()
);
#117=(
REPRESENTATION_RELATIONSHIP($,$,#12958,#12948)
REPRESENTATION_RELATIONSHIP_WITH_TRANSFORMATION(#60)
SHAPE_REPRESENTATION_RELATIONSHIP()
);
#118=(
REPRESENTATION_RELATIONSHIP($,$,#12965,#12964)
REPRESENTATION_RELATIONSHIP_WITH_TRANSFORMATION(#61)
SHAPE_REPRESENTATION_RELATIONSHIP()
);
#119=(
REPRESENTATION_RELATIONSHIP($,$,#12966,#12964)
REPRESENTATION_RELATIONSHIP_WITH_TRANSFORMATION(#62)
SHAPE_REPRESENTATION_RELATIONSHIP()
);
#120=(
REPRESENTATION_RELATIONSHIP($,$,#12967,#12964)
REPRESENTATION_RELATIONSHIP_WITH_TRANSFORMATION(#63)
SHAPE_REPRESENTATION_RELATIONSHIP()
);
#121=(
REPRESENTATION_RELATIONSHIP($,$,#12968,#12964)
REPRESENTATION_RELATIONSHIP_WITH_TRANSFORMATION(#64)
SHAPE_REPRESENTATION_RELATIONSHIP()
);
#122=(
REPRESENTATION_RELATIONSHIP($,$,#12969,#12964)
REPRESENTATION_RELATIONSHIP_WITH_TRANSFORMATION(#65)
SHAPE_REPRESENTATION_RELATIONSHIP()
);
#123=(
REPRESENTATION_RELATIONSHIP($,$,#12970,#12964)
REPRESENTATION_RELATIONSHIP_WITH_TRANSFORMATION(#66)
SHAPE_REPRESENTATION_RELATIONSHIP()
);
#124=(
REPRESENTATION_RELATIONSHIP($,$,#12971,#12964)
REPRESENTATION_RELATIONSHIP_WITH_TRANSFORMATION(#67)
SHAPE_REPRESENTATION_RELATIONSHIP()
);
#125=(
REPRESENTATION_RELATIONSHIP($,$,#12972,#12964)
REPRESENTATION_RELATIONSHIP_WITH_TRANSFORMATION(#68)
SHAPE_REPRESENTATION_RELATIONSHIP()
);
#126=(
REPRESENTATION_RELATIONSHIP($,$,#12973,#12964)
REPRESENTATION_RELATIONSHIP_WITH_TRANSFORMATION(#69)
SHAPE_REPRESENTATION_RELATIONSHIP()
);
#127=(
REPRESENTATION_RELATIONSHIP($,$,#12973,#12964)
REPRESENTATION_RELATIONSHIP_WITH_TRANSFORMATION(#70)
SHAPE_REPRESENTATION_RELATIONSHIP()
);
#128=(
REPRESENTATION_RELATIONSHIP($,$,#12932,#12931)
REPRESENTATION_RELATIONSHIP_WITH_TRANSFORMATION(#71)
SHAPE_REPRESENTATION_RELATIONSHIP()
);
#129=(
REPRESENTATION_RELATIONSHIP($,$,#12948,#12931)
REPRESENTATION_RELATIONSHIP_WITH_TRANSFORMATION(#72)
SHAPE_REPRESENTATION_RELATIONSHIP()
);
#130=(
REPRESENTATION_RELATIONSHIP($,$,#12964,#12931)
REPRESENTATION_RELATIONSHIP_WITH_TRANSFORMATION(#73)
SHAPE_REPRESENTATION_RELATIONSHIP()
);
#131=CONTEXT_DEPENDENT_SHAPE_REPRESENTATION(#74,#12846);
#132=CONTEXT_DEPENDENT_SHAPE_REPRESENTATION(#75,#12847);
#133=CONTEXT_DEPENDENT_SHAPE_REPRESENTATION(#76,#12848);
#134=CONTEXT_DEPENDENT_SHAPE_REPRESENTATION(#77,#12849);
#135=CONTEXT_DEPENDENT_SHAPE_REPRESENTATION(#78,#12850);
#136=CONTEXT_DEPENDENT_SHAPE_REPRESENTATION(#79,#12853);
#137=CONTEXT_DEPENDENT_SHAPE_REPRESENTATION(#80,#12854);
#138=CONTEXT_DEPENDENT_SHAPE_REPRESENTATION(#81,#12855);
#139=CONTEXT_DEPENDENT_SHAPE_REPRESENTATION(#82,#12856);
#140=CONTEXT_DEPENDENT_SHAPE_REPRESENTATION(#83,#12857);
#141=CONTEXT_DEPENDENT_SHAPE_REPRESENTATION(#84,#12858);
#142=CONTEXT_DEPENDENT_SHAPE_REPRESENTATION(#85,#12859);
#143=CONTEXT_DEPENDENT_SHAPE_REPRESENTATION(#86,#12860);
#144=CONTEXT_DEPENDENT_SHAPE_REPRESENTATION(#87,#12861);
#145=CONTEXT_DEPENDENT_SHAPE_REPRESENTATION(#88,#12862);
#146=CONTEXT_DEPENDENT_SHAPE_REPRESENTATION(#89,#12863);
#147=CONTEXT_DEPENDENT_SHAPE_REPRESENTATION(#90,#12864);
#148=CONTEXT_DEPENDENT_SHAPE_REPRESENTATION(#91,#12865);
#149=CONTEXT_DEPENDENT_SHAPE_REPRESENTATION(#92,#12866);
#150=CONTEXT_DEPENDENT_SHAPE_REPRESENTATION(#93,#12867);
#151=CONTEXT_DEPENDENT_SHAPE_REPRESENTATION(#94,#12868);
#152=CONTEXT_DEPENDENT_SHAPE_REPRESENTATION(#95,#12869);
#153=CONTEXT_DEPENDENT_SHAPE_REPRESENTATION(#96,#12870);
#154=CONTEXT_DEPENDENT_SHAPE_REPRESENTATION(#97,#12871);
#155=CONTEXT_DEPENDENT_SHAPE_REPRESENTATION(#98,#12872);
#156=CONTEXT_DEPENDENT_SHAPE_REPRESENTATION(#99,#12873);
#157=CONTEXT_DEPENDENT_SHAPE_REPRESENTATION(#100,#12890);
#158=CONTEXT_DEPENDENT_SHAPE_REPRESENTATION(#101,#12891);
#159=CONTEXT_DEPENDENT_SHAPE_REPRESENTATION(#102,#12892);
#160=CONTEXT_DEPENDENT_SHAPE_REPRESENTATION(#103,#12893);
#161=CONTEXT_DEPENDENT_SHAPE_REPRESENTATION(#104,#12894);
#162=CONTEXT_DEPENDENT_SHAPE_REPRESENTATION(#105,#12895);
#163=CONTEXT_DEPENDENT_SHAPE_REPRESENTATION(#106,#12896);
#164=CONTEXT_DEPENDENT_SHAPE_REPRESENTATION(#107,#12897);
#165=CONTEXT_DEPENDENT_SHAPE_REPRESENTATION(#108,#12898);
#166=CONTEXT_DEPENDENT_SHAPE_REPRESENTATION(#109,#12899);
#167=CONTEXT_DEPENDENT_SHAPE_REPRESENTATION(#110,#12900);
#168=CONTEXT_DEPENDENT_SHAPE_REPRESENTATION(#111,#12901);
#169=CONTEXT_DEPENDENT_SHAPE_REPRESENTATION(#112,#12902);
#170=CONTEXT_DEPENDENT_SHAPE_REPRESENTATION(#113,#12903);
#171=CONTEXT_DEPENDENT_SHAPE_REPRESENTATION(#114,#12904);
#172=CONTEXT_DEPENDENT_SHAPE_REPRESENTATION(#115,#12905);
#173=CONTEXT_DEPENDENT_SHAPE_REPRESENTATION(#116,#12906);
#174=CONTEXT_DEPENDENT_SHAPE_REPRESENTATION(#117,#12907);
#175=CONTEXT_DEPENDENT_SHAPE_REPRESENTATION(#118,#12918);
#176=CONTEXT_DEPENDENT_SHAPE_REPRESENTATION(#119,#12919);
#177=CONTEXT_DEPENDENT_SHAPE_REPRESENTATION(#120,#12920);
#178=CONTEXT_DEPENDENT_SHAPE_REPRESENTATION(#121,#12921);
#179=CONTEXT_DEPENDENT_SHAPE_REPRESENTATION(#122,#12922);
#180=CONTEXT_DEPENDENT_SHAPE_REPRESENTATION(#123,#12923);
#181=CONTEXT_DEPENDENT_SHAPE_REPRESENTATION(#124,#12924);
#182=CONTEXT_DEPENDENT_SHAPE_REPRESENTATION(#125,#12925);
#183=CONTEXT_DEPENDENT_SHAPE_REPRESENTATION(#126,#12926);
#184=CONTEXT_DEPENDENT_SHAPE_REPRESENTATION(#127,#12927);
#185=CONTEXT_DEPENDENT_SHAPE_REPRESENTATION(#128,#12928);
#186=CONTEXT_DEPENDENT_SHAPE_REPRESENTATION(#129,#12929);
#187=CONTEXT_DEPENDENT_SHAPE_REPRESENTATION(#130,#12930);
#188=NEXT_ASSEMBLY_USAGE_OCCURRENCE('Inner ring:1','Inner ring:1',
'Inner ring:1',#12984,#12985,'Inner ring:1');
#189=NEXT_ASSEMBLY_USAGE_OCCURRENCE('Outer ring:1','Outer ring:1',
'Outer ring:1',#12984,#12986,'Outer ring:1');
#190=NEXT_ASSEMBLY_USAGE_OCCURRENCE('Balls:1','Balls:1','Balls:1',#12984,
#12987,'Balls:1');
#191=NEXT_ASSEMBLY_USAGE_OCCURRENCE('Cage:1','Cage:1','Cage:1',#12984,#12988,
'Cage:1');
#192=NEXT_ASSEMBLY_USAGE_OCCURRENCE('Seals 2RS:1','Seals 2RS:1',
'Seals 2RS:1',#12984,#12989,'Seals 2RS:1');
#193=NEXT_ASSEMBLY_USAGE_OCCURRENCE('Base:1','Base:1','Base:1',#12976,#12977,
'Base:1');
#194=NEXT_ASSEMBLY_USAGE_OCCURRENCE('Bearing housing:1',
'Bearing housing:1','Bearing housing:1',#12976,#12978,
'Bearing housing:1');
#195=NEXT_ASSEMBLY_USAGE_OCCURRENCE('Outer race spacer:1',
'Outer race spacer:1','Outer race spacer:1',#12976,#12979,
'Outer race spacer:1');
#196=NEXT_ASSEMBLY_USAGE_OCCURRENCE('Bearing cap:1','Bearing cap:1',
'Bearing cap:1',#12976,#12980,'Bearing cap:1');
#197=NEXT_ASSEMBLY_USAGE_OCCURRENCE('Bearing cap (1):1',
'Bearing cap (1):1','Bearing cap (1):1',#12976,#12981,
'Bearing cap (1):1');
#198=NEXT_ASSEMBLY_USAGE_OCCURRENCE('Bonded foot:1','Bonded foot:1',
'Bonded foot:1',#12976,#12982,'Bonded foot:1');
#199=NEXT_ASSEMBLY_USAGE_OCCURRENCE('Bonded foot (1):1',
'Bonded foot (1):1','Bonded foot (1):1',#12976,#12983,
'Bonded foot (1):1');
#200=NEXT_ASSEMBLY_USAGE_OCCURRENCE(
'Sealed Ball Bearing - 25 x 52 x 15 mm:2',
'Sealed Ball Bearing - 25 x 52 x 15 mm:2',
'Sealed Ball Bearing - 25 x 52 x 15 mm:2',#12976,#12984,
'Sealed Ball Bearing - 25 x 52 x 15 mm:2');
#201=NEXT_ASSEMBLY_USAGE_OCCURRENCE('Cap Screw - M6x25:2',
'Cap Screw - M6x25:2','Cap Screw - M6x25:2',#12976,#12990,
'Cap Screw - M6x25:2');
#202=NEXT_ASSEMBLY_USAGE_OCCURRENCE('Cap Screw - M6x25:3',
'Cap Screw - M6x25:3','Cap Screw - M6x25:3',#12976,#12990,
'Cap Screw - M6x25:3');
#203=NEXT_ASSEMBLY_USAGE_OCCURRENCE(
'Sealed Ball Bearing - 25 x 52 x 15 mm:3',
'Sealed Ball Bearing - 25 x 52 x 15 mm:3',
'Sealed Ball Bearing - 25 x 52 x 15 mm:3',#12976,#12984,
'Sealed Ball Bearing - 25 x 52 x 15 mm:3');
#204=NEXT_ASSEMBLY_USAGE_OCCURRENCE('Cap Screw - M6x25:4',
'Cap Screw - M6x25:4','Cap Screw - M6x25:4',#12976,#12990,
'Cap Screw - M6x25:4');
#205=NEXT_ASSEMBLY_USAGE_OCCURRENCE('Cap Screw - M6x25:5',
'Cap Screw - M6x25:5','Cap Screw - M6x25:5',#12976,#12990,
'Cap Screw - M6x25:5');
#206=NEXT_ASSEMBLY_USAGE_OCCURRENCE('Cap Screw - M4x16:2',
'Cap Screw - M4x16:2','Cap Screw - M4x16:2',#12976,#12991,
'Cap Screw - M4x16:2');
#207=NEXT_ASSEMBLY_USAGE_OCCURRENCE('Cap Screw - M4x16:3',
'Cap Screw - M4x16:3','Cap Screw - M4x16:3',#12976,#12991,
'Cap Screw - M4x16:3');
#208=NEXT_ASSEMBLY_USAGE_OCCURRENCE('Cap Screw - M4x16:4',
'Cap Screw - M4x16:4','Cap Screw - M4x16:4',#12976,#12991,
'Cap Screw - M4x16:4');
#209=NEXT_ASSEMBLY_USAGE_OCCURRENCE('Cap Screw - M4x16:5',
'Cap Screw - M4x16:5','Cap Screw - M4x16:5',#12976,#12991,
'Cap Screw - M4x16:5');
#210=NEXT_ASSEMBLY_USAGE_OCCURRENCE('Cap Screw - M4x16:6',
'Cap Screw - M4x16:6','Cap Screw - M4x16:6',#12976,#12991,
'Cap Screw - M4x16:6');
#211=NEXT_ASSEMBLY_USAGE_OCCURRENCE('Cap Screw - M4x16:7',
'Cap Screw - M4x16:7','Cap Screw - M4x16:7',#12976,#12991,
'Cap Screw - M4x16:7');
#212=NEXT_ASSEMBLY_USAGE_OCCURRENCE('Cap Screw - M4x16:8',
'Cap Screw - M4x16:8','Cap Screw - M4x16:8',#12976,#12991,
'Cap Screw - M4x16:8');
#213=NEXT_ASSEMBLY_USAGE_OCCURRENCE('Cap Screw - M4x16:9',
'Cap Screw - M4x16:9','Cap Screw - M4x16:9',#12976,#12991,
'Cap Screw - M4x16:9');
#214=NEXT_ASSEMBLY_USAGE_OCCURRENCE('Inner ring (1):1',
'Inner ring (1):1','Inner ring (1):1',#13002,#13003,'Inner ring (1):1');
#215=NEXT_ASSEMBLY_USAGE_OCCURRENCE('Outer ring (1):1',
'Outer ring (1):1','Outer ring (1):1',#13002,#13004,'Outer ring (1):1');
#216=NEXT_ASSEMBLY_USAGE_OCCURRENCE('Balls (1):1','Balls (1):1',
'Balls (1):1',#13002,#13005,'Balls (1):1');
#217=NEXT_ASSEMBLY_USAGE_OCCURRENCE('Cage (1):1','Cage (1):1',
'Cage (1):1',#13002,#13006,'Cage (1):1');
#218=NEXT_ASSEMBLY_USAGE_OCCURRENCE('Seals 2RS (1):1','Seals 2RS (1):1',
'Seals 2RS (1):1',#13002,#13007,'Seals 2RS (1):1');
#219=NEXT_ASSEMBLY_USAGE_OCCURRENCE('Shaft:1','Shaft:1','Shaft:1',#12992,
#12993,'Shaft:1');
#220=NEXT_ASSEMBLY_USAGE_OCCURRENCE('Inner race spacer:1',
'Inner race spacer:1','Inner race spacer:1',#12992,#12994,
'Inner race spacer:1');
#221=NEXT_ASSEMBLY_USAGE_OCCURRENCE('Shaft collar:1','Shaft collar:1',
'Shaft collar:1',#12992,#12995,'Shaft collar:1');
#222=NEXT_ASSEMBLY_USAGE_OCCURRENCE('Square drive adapter:1',
'Square drive adapter:1','Square drive adapter:1',#12992,#12996,
'Square drive adapter:1');
#223=NEXT_ASSEMBLY_USAGE_OCCURRENCE('Torque arm:1','Torque arm:1',
'Torque arm:1',#12992,#12997,'Torque arm:1');
#224=NEXT_ASSEMBLY_USAGE_OCCURRENCE('Hanger bearing retainer:1',
'Hanger bearing retainer:1','Hanger bearing retainer:1',#12992,#12998,
'Hanger bearing retainer:1');
#225=NEXT_ASSEMBLY_USAGE_OCCURRENCE('Hanger bearing retainer (1):1',
'Hanger bearing retainer (1):1','Hanger bearing retainer (1):1',#12992,
#12999,'Hanger bearing retainer (1):1');
#226=NEXT_ASSEMBLY_USAGE_OCCURRENCE('Key 8x7x20:2','Key 8x7x20:2',
'Key 8x7x20:2',#12992,#13000,'Key 8x7x20:2');
#227=NEXT_ASSEMBLY_USAGE_OCCURRENCE('Key 8x7x20:3','Key 8x7x20:3',
'Key 8x7x20:3',#12992,#13000,'Key 8x7x20:3');
#228=NEXT_ASSEMBLY_USAGE_OCCURRENCE('Socket Set Screw - M5x8:2',
'Socket Set Screw - M5x8:2','Socket Set Screw - M5x8:2',#12992,#13001,
'Socket Set Screw - M5x8:2');
#229=NEXT_ASSEMBLY_USAGE_OCCURRENCE('Socket Set Screw - M5x8:3',
'Socket Set Screw - M5x8:3','Socket Set Screw - M5x8:3',#12992,#13001,
'Socket Set Screw - M5x8:3');
#230=NEXT_ASSEMBLY_USAGE_OCCURRENCE('Socket Set Screw - M5x8:4',
'Socket Set Screw - M5x8:4','Socket Set Screw - M5x8:4',#12992,#13001,
'Socket Set Screw - M5x8:4');
#231=NEXT_ASSEMBLY_USAGE_OCCURRENCE(
'Sealed Ball Bearing - 10 x 30 x 9 mm:2',
'Sealed Ball Bearing - 10 x 30 x 9 mm:2',
'Sealed Ball Bearing - 10 x 30 x 9 mm:2',#12992,#13002,
'Sealed Ball Bearing - 10 x 30 x 9 mm:2');
#232=NEXT_ASSEMBLY_USAGE_OCCURRENCE('Weight hanger:1','Weight hanger:1',
'Weight hanger:1',#13008,#13009,'Weight hanger:1');
#233=NEXT_ASSEMBLY_USAGE_OCCURRENCE('Hanger axle:1','Hanger axle:1',
'Hanger axle:1',#13008,#13010,'Hanger axle:1');
#234=NEXT_ASSEMBLY_USAGE_OCCURRENCE('Hanger inner spacer:1',
'Hanger inner spacer:1','Hanger inner spacer:1',#13008,#13011,
'Hanger inner spacer:1');
#235=NEXT_ASSEMBLY_USAGE_OCCURRENCE('Hanger inner spacer (1):1',
'Hanger inner spacer (1):1','Hanger inner spacer (1):1',#13008,#13012,
'Hanger inner spacer (1):1');
#236=NEXT_ASSEMBLY_USAGE_OCCURRENCE('Hanger outer shim:1',
'Hanger outer shim:1','Hanger outer shim:1',#13008,#13013,
'Hanger outer shim:1');
#237=NEXT_ASSEMBLY_USAGE_OCCURRENCE('Hanger outer shim (1):1',
'Hanger outer shim (1):1','Hanger outer shim (1):1',#13008,#13014,
'Hanger outer shim (1):1');
#238=NEXT_ASSEMBLY_USAGE_OCCURRENCE('Hanger keeper:1','Hanger keeper:1',
'Hanger keeper:1',#13008,#13015,'Hanger keeper:1');
#239=NEXT_ASSEMBLY_USAGE_OCCURRENCE('Hanger keeper (1):1',
'Hanger keeper (1):1','Hanger keeper (1):1',#13008,#13016,
'Hanger keeper (1):1');
#240=NEXT_ASSEMBLY_USAGE_OCCURRENCE('M4x10 Cap Screw:2',
'M4x10 Cap Screw:2','M4x10 Cap Screw:2',#13008,#13017,
'M4x10 Cap Screw:2');
#241=NEXT_ASSEMBLY_USAGE_OCCURRENCE('M4x10 Cap Screw:3',
'M4x10 Cap Screw:3','M4x10 Cap Screw:3',#13008,#13017,
'M4x10 Cap Screw:3');
#242=NEXT_ASSEMBLY_USAGE_OCCURRENCE('Bearing stand:1','Bearing stand:1',
'Bearing stand:1',#12975,#12976,'Bearing stand:1');
#243=NEXT_ASSEMBLY_USAGE_OCCURRENCE('Shaft and torque arm:1',
'Shaft and torque arm:1','Shaft and torque arm:1',#12975,#12992,
'Shaft and torque arm:1');
#244=NEXT_ASSEMBLY_USAGE_OCCURRENCE('Weight hanger (1):1',
'Weight hanger (1):1','Weight hanger (1):1',#12975,#13008,
'Weight hanger (1):1');
#245=B_SPLINE_CURVE_WITH_KNOTS('',3,(#10516,#10517,#10518,#10519,#10520,
#10521,#10522,#10523,#10524,#10525,#10526,#10527,#10528,#10529,#10530,#10531,
#10532,#10533,#10534,#10535,#10536,#10537),.UNSPECIFIED.,.F.,.F.,(4,2,2,
2,2,2,2,2,2,2,4),(0.0789043916784349,0.21052649634152,0.31578974451228,
0.421052992683041,0.522171766675512,0.623290540667983,0.724409314660453,
0.825528088652924,0.930791336823684,1.03605458499444,1.16767668965753),
 .UNSPECIFIED.);
#246=B_SPLINE_CURVE_WITH_KNOTS('',3,(#10541,#10542,#10543,#10544,#10545,
#10546,#10547,#10548,#10549,#10550,#10551,#10552,#10553,#10554,#10555,#10556,
#10557,#10558,#10559,#10560,#10561,#10562),.UNSPECIFIED.,.F.,.F.,(4,2,2,
2,2,2,2,2,2,2,4),(0.0774711646211702,0.142095081356994,0.284190162713987,
0.410912155766437,0.514012992401139,0.617113829035841,0.720214665670543,
0.823315502305246,0.950037495357694,1.09213257671469,1.15675649345051),
 .UNSPECIFIED.);
#247=B_SPLINE_CURVE_WITH_KNOTS('',3,(#10568,#10569,#10570,#10571,#10572,
#10573,#10574,#10575,#10576,#10577,#10578,#10579,#10580,#10581,#10582,#10583,
#10584,#10585,#10586,#10587,#10588,#10589),.UNSPECIFIED.,.F.,.F.,(4,2,2,
2,2,2,2,2,2,2,4),(0.0774711646211703,0.142095081356994,0.284190162713988,
0.410912155766436,0.514012992401139,0.617113829035841,0.720214665670544,
0.823315502305246,0.950037495357695,1.09213257671469,1.15675649345051),
 .UNSPECIFIED.);
#248=B_SPLINE_CURVE_WITH_KNOTS('',3,(#10593,#10594,#10595,#10596,#10597,
#10598,#10599,#10600,#10601,#10602,#10603,#10604,#10605,#10606,#10607,#10608,
#10609,#10610,#10611,#10612,#10613,#10614),.UNSPECIFIED.,.F.,.F.,(4,2,2,
2,2,2,2,2,2,2,4),(0.0774711646211702,0.142095081356994,0.284190162713988,
0.410912155766436,0.514012992401139,0.617113829035841,0.720214665670544,
0.823315502305246,0.950037495357695,1.09213257671469,1.15675649345051),
 .UNSPECIFIED.);
#249=B_SPLINE_CURVE_WITH_KNOTS('',3,(#10618,#10619,#10620,#10621,#10622,
#10623,#10624,#10625,#10626,#10627,#10628,#10629,#10630,#10631,#10632,#10633,
#10634,#10635,#10636,#10637,#10638,#10639),.UNSPECIFIED.,.F.,.F.,(4,2,2,
2,2,2,2,2,2,2,4),(0.0774711646211702,0.142095081356994,0.284190162713988,
0.410912155766436,0.514012992401139,0.617113829035842,0.720214665670544,
0.823315502305246,0.950037495357696,1.09213257671469,1.15675649345051),
 .UNSPECIFIED.);
#250=B_SPLINE_CURVE_WITH_KNOTS('',3,(#10648,#10649,#10650,#10651,#10652,
#10653,#10654,#10655,#10656,#10657,#10658,#10659,#10660,#10661,#10662,#10663,
#10664,#10665,#10666,#10667,#10668,#10669),.UNSPECIFIED.,.F.,.F.,(4,2,2,
2,2,2,2,2,2,2,4),(0.0774711646211702,0.142095081356994,0.284190162713987,
0.410912155766436,0.514012992401139,0.617113829035841,0.720214665670543,
0.823315502305246,0.950037495357695,1.09213257671469,1.15675649345051),
 .UNSPECIFIED.);
#251=B_SPLINE_CURVE_WITH_KNOTS('',3,(#10673,#10674,#10675,#10676,#10677,
#10678,#10679,#10680,#10681,#10682,#10683,#10684,#10685,#10686,#10687,#10688,
#10689,#10690,#10691,#10692,#10693,#10694),.UNSPECIFIED.,.F.,.F.,(4,2,2,
2,2,2,2,2,2,2,4),(0.0774711646211702,0.142095081356994,0.284190162713987,
0.410912155766436,0.514012992401139,0.617113829035841,0.720214665670543,
0.823315502305246,0.950037495357695,1.09213257671469,1.15675649345051),
 .UNSPECIFIED.);
#252=B_SPLINE_CURVE_WITH_KNOTS('',3,(#10698,#10699,#10700,#10701,#10702,
#10703,#10704,#10705,#10706,#10707,#10708,#10709,#10710,#10711,#10712,#10713,
#10714,#10715,#10716,#10717,#10718,#10719),.UNSPECIFIED.,.F.,.F.,(4,2,2,
2,2,2,2,2,2,2,4),(0.0774711646211703,0.142095081356994,0.284190162713988,
0.410912155766437,0.514012992401139,0.617113829035841,0.720214665670544,
0.823315502305247,0.950037495357696,1.09213257671469,1.15675649345051),
 .UNSPECIFIED.);
#253=B_SPLINE_CURVE_WITH_KNOTS('',3,(#10723,#10724,#10725,#10726,#10727,
#10728,#10729,#10730,#10731,#10732,#10733,#10734,#10735,#10736,#10737,#10738,
#10739,#10740,#10741,#10742,#10743,#10744),.UNSPECIFIED.,.F.,.F.,(4,2,2,
2,2,2,2,2,2,2,4),(0.0774711646211703,0.142095081356994,0.284190162713987,
0.410912155766436,0.514012992401139,0.617113829035841,0.720214665670543,
0.823315502305245,0.950037495357694,1.09213257671469,1.15675649345051),
 .UNSPECIFIED.);
#254=B_SPLINE_CURVE_WITH_KNOTS('',3,(#10748,#10749,#10750,#10751,#10752,
#10753,#10754,#10755,#10756,#10757,#10758,#10759,#10760,#10761,#10762,#10763,
#10764,#10765,#10766,#10767,#10768,#10769),.UNSPECIFIED.,.F.,.F.,(4,2,2,
2,2,2,2,2,2,2,4),(0.0774711646211703,0.142095081356994,0.284190162713988,
0.410912155766437,0.514012992401139,0.617113829035841,0.720214665670544,
0.823315502305246,0.950037495357695,1.09213257671469,1.15675649345051),
 .UNSPECIFIED.);
#255=B_SPLINE_CURVE_WITH_KNOTS('',3,(#10777,#10778,#10779,#10780,#10781,
#10782,#10783,#10784,#10785,#10786,#10787,#10788,#10789,#10790,#10791,#10792,
#10793,#10794,#10795,#10796,#10797,#10798),.UNSPECIFIED.,.F.,.F.,(4,2,2,
2,2,2,2,2,2,2,4),(0.0789043916784349,0.21052649634152,0.315789744512281,
0.421052992683041,0.522171766675512,0.623290540667983,0.724409314660453,
0.825528088652924,0.930791336823684,1.03605458499444,1.16767668965753),
 .UNSPECIFIED.);
#256=B_SPLINE_CURVE_WITH_KNOTS('',3,(#10806,#10807,#10808,#10809,#10810,
#10811,#10812,#10813,#10814,#10815,#10816,#10817,#10818,#10819,#10820,#10821,
#10822,#10823,#10824,#10825,#10826,#10827),.UNSPECIFIED.,.F.,.F.,(4,2,2,
2,2,2,2,2,2,2,4),(0.0789043916784348,0.210526496341521,0.315789744512281,
0.421052992683042,0.522171766675513,0.623290540667983,0.724409314660454,
0.825528088652925,0.930791336823685,1.03605458499444,1.16767668965753),
 .UNSPECIFIED.);
#257=B_SPLINE_CURVE_WITH_KNOTS('',3,(#10835,#10836,#10837,#10838,#10839,
#10840,#10841,#10842,#10843,#10844,#10845,#10846,#10847,#10848,#10849,#10850,
#10851,#10852,#10853,#10854,#10855,#10856),.UNSPECIFIED.,.F.,.F.,(4,2,2,
2,2,2,2,2,2,2,4),(0.0789043916784349,0.21052649634152,0.31578974451228,
0.421052992683041,0.522171766675511,0.623290540667982,0.724409314660453,
0.825528088652924,0.930791336823685,1.03605458499444,1.16767668965753),
 .UNSPECIFIED.);
#258=B_SPLINE_CURVE_WITH_KNOTS('',3,(#10866,#10867,#10868,#10869,#10870,
#10871,#10872,#10873,#10874,#10875,#10876,#10877,#10878,#10879,#10880,#10881,
#10882,#10883,#10884,#10885,#10886,#10887),.UNSPECIFIED.,.F.,.F.,(4,2,2,
2,2,2,2,2,2,2,4),(0.0789043916784348,0.21052649634152,0.315789744512281,
0.421052992683041,0.522171766675511,0.623290540667982,0.724409314660453,
0.825528088652924,0.930791336823684,1.03605458499444,1.16767668965753),
 .UNSPECIFIED.);
#259=B_SPLINE_CURVE_WITH_KNOTS('',3,(#10895,#10896,#10897,#10898,#10899,
#10900,#10901,#10902,#10903,#10904,#10905,#10906,#10907,#10908,#10909,#10910,
#10911,#10912,#10913,#10914,#10915,#10916),.UNSPECIFIED.,.F.,.F.,(4,2,2,
2,2,2,2,2,2,2,4),(0.0789043916784348,0.21052649634152,0.31578974451228,
0.42105299268304,0.522171766675511,0.623290540667982,0.724409314660453,
0.825528088652924,0.930791336823684,1.03605458499444,1.16767668965753),
 .UNSPECIFIED.);
#260=B_SPLINE_CURVE_WITH_KNOTS('',3,(#10924,#10925,#10926,#10927,#10928,
#10929,#10930,#10931,#10932,#10933,#10934,#10935,#10936,#10937,#10938,#10939,
#10940,#10941,#10942,#10943,#10944,#10945),.UNSPECIFIED.,.F.,.F.,(4,2,2,
2,2,2,2,2,2,2,4),(0.0789043916784348,0.21052649634152,0.315789744512281,
0.421052992683041,0.522171766675512,0.623290540667982,0.724409314660453,
0.825528088652924,0.930791336823684,1.03605458499444,1.16767668965753),
 .UNSPECIFIED.);
#261=B_SPLINE_CURVE_WITH_KNOTS('',3,(#10953,#10954,#10955,#10956,#10957,
#10958,#10959,#10960,#10961,#10962,#10963,#10964,#10965,#10966,#10967,#10968,
#10969,#10970,#10971,#10972,#10973,#10974),.UNSPECIFIED.,.F.,.F.,(4,2,2,
2,2,2,2,2,2,2,4),(0.0789043916784349,0.21052649634152,0.31578974451228,
0.42105299268304,0.522171766675511,0.623290540667982,0.724409314660453,
0.825528088652924,0.930791336823684,1.03605458499444,1.16767668965753),
 .UNSPECIFIED.);
#262=B_SPLINE_CURVE_WITH_KNOTS('',3,(#10983,#10984,#10985,#10986,#10987,
#10988,#10989,#10990,#10991,#10992,#10993,#10994,#10995,#10996,#10997,#10998,
#10999,#11000,#11001,#11002,#11003,#11004),.UNSPECIFIED.,.F.,.F.,(4,2,2,
2,2,2,2,2,2,2,4),(0.0789043916784348,0.21052649634152,0.31578974451228,
0.42105299268304,0.522171766675511,0.623290540667982,0.724409314660453,
0.825528088652924,0.930791336823684,1.03605458499444,1.16767668965753),
 .UNSPECIFIED.);
#263=B_SPLINE_CURVE_WITH_KNOTS('',3,(#11304,#11305,#11306,#11307,#11308,
#11309,#11310,#11311,#11312,#11313,#11314,#11315,#11316,#11317),
 .UNSPECIFIED.,.F.,.F.,(4,2,2,2,2,2,4),(0.714680326757342,0.79264866270072,
0.871912238073927,0.951175813447134,1.03043938882034,1.10970296419355,1.18767130013693),
 .UNSPECIFIED.);
#264=B_SPLINE_CURVE_WITH_KNOTS('',3,(#11323,#11324,#11325,#11326,#11327,
#11328,#11329,#11330,#11331,#11332,#11333,#11334,#11335,#11336,#11337,#11338,
#11339,#11340),.UNSPECIFIED.,.F.,.F.,(4,2,2,2,2,2,2,2,4),(0.,0.0791819055472369,
0.158363811094474,0.237545215630596,0.316726620166718,0.395908024702839,
0.475089429238961,0.554271334786198,0.633453240333435),.UNSPECIFIED.);
#265=B_SPLINE_CURVE_WITH_KNOTS('',3,(#11341,#11342,#11343,#11344,#11345,
#11346,#11347,#11348,#11349,#11350,#11351,#11352,#11353,#11354,#11355,#11356,
#11357,#11358),.UNSPECIFIED.,.F.,.F.,(4,2,2,2,2,2,2,2,4),(0.633453240333435,
0.712635145880672,0.791817051427908,0.87099845596403,0.950179860500152,
1.02936126503627,1.1085426695724,1.18772457511963,1.26690648066687),
 .UNSPECIFIED.);
#266=B_SPLINE_CURVE_WITH_KNOTS('',3,(#11361,#11362,#11363,#11364,#11365,
#11366,#11367,#11368,#11369,#11370,#11371,#11372,#11373,#11374),
 .UNSPECIFIED.,.F.,.F.,(4,2,2,2,2,2,4),(0.080563117792587,0.158531453735964,
0.237795029109171,0.317058604482378,0.396322179855585,0.475585755228792,
0.553554091172169),.UNSPECIFIED.);
#267=B_SPLINE_CURVE_WITH_KNOTS('',3,(#11399,#11400,#11401,#11402,#11403,
#11404,#11405,#11406,#11407,#11408,#11409,#11410,#11411,#11412),
 .UNSPECIFIED.,.F.,.F.,(4,2,2,2,2,2,4),(0.779149138325151,0.792661737650614,
0.87192659943798,0.951191461225345,1.03045632301271,1.10972118480008,1.12323378412554),
 .UNSPECIFIED.);
#268=B_SPLINE_CURVE_WITH_KNOTS('',3,(#11418,#11419,#11420,#11421,#11422,
#11423,#11424,#11425,#11426,#11427,#11428,#11429,#11430,#11431,#11432,#11433,
#11434,#11435),.UNSPECIFIED.,.F.,.F.,(4,2,2,2,2,2,2,2,4),(0.,0.0791670250779304,
0.158334050155861,0.237500747381212,0.316667444606564,0.395834141831915,
0.475000839057267,0.554167864135197,0.633334889213128),.UNSPECIFIED.);
#269=B_SPLINE_CURVE_WITH_KNOTS('',3,(#11436,#11437,#11438,#11439,#11440,
#11441,#11442,#11443,#11444,#11445,#11446,#11447,#11448,#11449,#11450,#11451,
#11452,#11453),.UNSPECIFIED.,.F.,.F.,(4,2,2,2,2,2,2,2,4),(0.633334889213128,
0.712501914291058,0.791668939368988,0.87083563659434,0.950002333819691,
1.02916903104504,1.10833572827039,1.18750275334832,1.26666977842626),
 .UNSPECIFIED.);
#270=B_SPLINE_CURVE_WITH_KNOTS('',3,(#11456,#11457,#11458,#11459,#11460,
#11461,#11462,#11463,#11464,#11465,#11466,#11467,#11468,#11469),
 .UNSPECIFIED.,.F.,.F.,(4,2,2,2,2,2,4),(0.145021497508255,0.158534096833718,
0.237798958621083,0.317063820408448,0.396328682195814,0.475593543983179,
0.489106143308642),.UNSPECIFIED.);
#271=B_SPLINE_CURVE_WITH_KNOTS('',3,(#11550,#11551,#11552,#11553,#11554,
#11555,#11556,#11557,#11558,#11559,#11560,#11561,#11562,#11563),
 .UNSPECIFIED.,.F.,.F.,(4,2,2,2,2,2,4),(0.779149138325153,0.792661737650616,
0.871926599437981,0.951191461225347,1.03045632301271,1.10972118480008,1.12323378412554),
 .UNSPECIFIED.);
#272=B_SPLINE_CURVE_WITH_KNOTS('',3,(#11569,#11570,#11571,#11572,#11573,
#11574,#11575,#11576,#11577,#11578,#11579,#11580,#11581,#11582,#11583,#11584,
#11585,#11586),.UNSPECIFIED.,.F.,.F.,(4,2,2,2,2,2,2,2,4),(0.,0.0791442954208927,
0.158288590841785,0.23743275251224,0.316576914182695,0.39572107585315,0.474865237523604,
0.554009532944497,0.63315382836539),.UNSPECIFIED.);
#273=B_SPLINE_CURVE_WITH_KNOTS('',3,(#11587,#11588,#11589,#11590,#11591,
#11592,#11593,#11594,#11595,#11596,#11597,#11598,#11599,#11600,#11601,#11602,
#11603,#11604),.UNSPECIFIED.,.F.,.F.,(4,2,2,2,2,2,2,2,4),(0.63315382836539,
0.712298123786282,0.791442419207175,0.87058658087763,0.949730742548085,
1.02887490421854,1.10801906588899,1.18716336130989,1.26630765673078),
 .UNSPECIFIED.);
#274=B_SPLINE_CURVE_WITH_KNOTS('',3,(#11607,#11608,#11609,#11610,#11611,
#11612,#11613,#11614,#11615,#11616,#11617,#11618,#11619,#11620),
 .UNSPECIFIED.,.F.,.F.,(4,2,2,2,2,2,4),(0.145021497508257,0.158534096833718,
0.237798958621084,0.317063820408449,0.396328682195814,0.47559354398318,
0.489106143308642),.UNSPECIFIED.);
#275=B_SPLINE_CURVE_WITH_KNOTS('',3,(#11943,#11944,#11945,#11946,#11947,
#11948,#11949,#11950,#11951,#11952,#11953,#11954,#11955,#11956,#11957,#11958,
#11959,#11960,#11961,#11962,#11963,#11964),.UNSPECIFIED.,.F.,.F.,(4,2,2,
2,2,2,2,2,2,2,4),(0.0473477652366656,0.126350602536658,0.189525903804987,
0.252701205073317,0.313298422430275,0.373895639787233,0.434492857144191,
0.495090074501149,0.558265375769478,0.621440677037807,0.7004435143378),
 .UNSPECIFIED.);
#276=B_SPLINE_CURVE_WITH_KNOTS('',3,(#11968,#11969,#11970,#11971,#11972,
#11973,#11974,#11975,#11976,#11977,#11978,#11979,#11980,#11981,#11982,#11983,
#11984,#11985,#11986,#11987,#11988,#11989),.UNSPECIFIED.,.F.,.F.,(4,2,2,
2,2,2,2,2,2,2,4),(0.0464897534940957,0.0852567806515119,0.170513561303024,
0.246687263103517,0.308657850341199,0.370628437578881,0.432599024816563,
0.494569612054245,0.570743313854739,0.656000094506251,0.694767121663666),
 .UNSPECIFIED.);
#277=B_SPLINE_CURVE_WITH_KNOTS('',3,(#11995,#11996,#11997,#11998,#11999,
#12000,#12001,#12002,#12003,#12004,#12005,#12006,#12007,#12008,#12009,#12010,
#12011,#12012,#12013,#12014,#12015,#12016),.UNSPECIFIED.,.F.,.F.,(4,2,2,
2,2,2,2,2,2,2,4),(0.0464897534940957,0.0852567806515118,0.170513561303024,
0.246687263103517,0.308657850341199,0.370628437578881,0.432599024816563,
0.494569612054245,0.570743313854738,0.65600009450625,0.694767121663666),
 .UNSPECIFIED.);
#278=B_SPLINE_CURVE_WITH_KNOTS('',3,(#12020,#12021,#12022,#12023,#12024,
#12025,#12026,#12027,#12028,#12029,#12030,#12031,#12032,#12033,#12034,#12035,
#12036,#12037,#12038,#12039,#12040,#12041),.UNSPECIFIED.,.F.,.F.,(4,2,2,
2,2,2,2,2,2,2,4),(0.0464897534940957,0.0852567806515119,0.170513561303024,
0.246687263103517,0.308657850341199,0.370628437578881,0.432599024816563,
0.494569612054245,0.570743313854739,0.656000094506251,0.694767121663666),
 .UNSPECIFIED.);
#279=B_SPLINE_CURVE_WITH_KNOTS('',3,(#12045,#12046,#12047,#12048,#12049,
#12050,#12051,#12052,#12053,#12054,#12055,#12056),.UNSPECIFIED.,.F.,.F.,
(4,2,2,2,2,4),(0.0464897534940957,0.0852567806515119,0.170513561303024,
0.246687263103517,0.308657850341199,0.370628437578881),.UNSPECIFIED.);
#280=B_SPLINE_CURVE_WITH_KNOTS('',3,(#12061,#12062,#12063,#12064,#12065,
#12066,#12067,#12068,#12069,#12070,#12071,#12072),.UNSPECIFIED.,.F.,.F.,
(4,2,2,2,2,4),(0.370628437578881,0.432599024816563,0.494569612054245,0.570743313854738,
0.65600009450625,0.694767121663666),.UNSPECIFIED.);
#281=B_SPLINE_CURVE_WITH_KNOTS('',3,(#12076,#12077,#12078,#12079,#12080,
#12081,#12082,#12083,#12084,#12085,#12086,#12087,#12088,#12089,#12090,#12091,
#12092,#12093,#12094,#12095,#12096,#12097),.UNSPECIFIED.,.F.,.F.,(4,2,2,
2,2,2,2,2,2,2,4),(0.0464897534940957,0.0852567806515121,0.170513561303024,
0.246687263103518,0.308657850341199,0.370628437578881,0.432599024816563,
0.494569612054245,0.570743313854738,0.65600009450625,0.694767121663666),
 .UNSPECIFIED.);
#282=B_SPLINE_CURVE_WITH_KNOTS('',3,(#12101,#12102,#12103,#12104,#12105,
#12106,#12107,#12108,#12109,#12110,#12111,#12112,#12113,#12114,#12115,#12116,
#12117,#12118,#12119,#12120,#12121,#12122),.UNSPECIFIED.,.F.,.F.,(4,2,2,
2,2,2,2,2,2,2,4),(0.0464897534940957,0.0852567806515119,0.170513561303024,
0.246687263103517,0.308657850341199,0.370628437578881,0.432599024816563,
0.494569612054245,0.570743313854738,0.65600009450625,0.694767121663667),
 .UNSPECIFIED.);
#283=B_SPLINE_CURVE_WITH_KNOTS('',3,(#12126,#12127,#12128,#12129,#12130,
#12131,#12132,#12133,#12134,#12135,#12136,#12137,#12138,#12139,#12140,#12141,
#12142,#12143,#12144,#12145,#12146,#12147),.UNSPECIFIED.,.F.,.F.,(4,2,2,
2,2,2,2,2,2,2,4),(0.0464897534940957,0.0852567806515119,0.170513561303024,
0.246687263103517,0.308657850341199,0.370628437578881,0.432599024816563,
0.494569612054245,0.570743313854738,0.65600009450625,0.694767121663666),
 .UNSPECIFIED.);
#284=B_SPLINE_CURVE_WITH_KNOTS('',3,(#12151,#12152,#12153,#12154,#12155,
#12156,#12157,#12158,#12159,#12160,#12161,#12162,#12163,#12164,#12165,#12166,
#12167,#12168,#12169,#12170,#12171,#12172),.UNSPECIFIED.,.F.,.F.,(4,2,2,
2,2,2,2,2,2,2,4),(0.0464897534940957,0.0852567806515119,0.170513561303024,
0.246687263103517,0.308657850341199,0.370628437578881,0.432599024816563,
0.494569612054245,0.570743313854739,0.656000094506251,0.694767121663667),
 .UNSPECIFIED.);
#285=B_SPLINE_CURVE_WITH_KNOTS('',3,(#12180,#12181,#12182,#12183,#12184,
#12185,#12186,#12187,#12188,#12189,#12190,#12191,#12192,#12193,#12194,#12195,
#12196,#12197,#12198,#12199,#12200,#12201),.UNSPECIFIED.,.F.,.F.,(4,2,2,
2,2,2,2,2,2,2,4),(0.0473477652366656,0.126350602536658,0.189525903804987,
0.252701205073316,0.313298422430274,0.373895639787232,0.434492857144191,
0.495090074501149,0.558265375769478,0.621440677037807,0.7004435143378),
 .UNSPECIFIED.);
#286=B_SPLINE_CURVE_WITH_KNOTS('',3,(#12209,#12210,#12211,#12212,#12213,
#12214,#12215,#12216,#12217,#12218,#12219,#12220,#12221,#12222,#12223,#12224,
#12225,#12226,#12227,#12228,#12229,#12230),.UNSPECIFIED.,.F.,.F.,(4,2,2,
2,2,2,2,2,2,2,4),(0.0473477652366656,0.126350602536658,0.189525903804987,
0.252701205073317,0.313298422430275,0.373895639787233,0.434492857144191,
0.495090074501149,0.558265375769478,0.621440677037807,0.7004435143378),
 .UNSPECIFIED.);
#287=B_SPLINE_CURVE_WITH_KNOTS('',3,(#12239,#12240,#12241,#12242,#12243,
#12244,#12245,#12246,#12247,#12248,#12249,#12250),.UNSPECIFIED.,.F.,.F.,
(4,2,2,2,2,4),(0.0473477652366656,0.126350602536658,0.189525903804987,0.252701205073316,
0.313298422430275,0.373895639787233),.UNSPECIFIED.);
#288=B_SPLINE_CURVE_WITH_KNOTS('',3,(#12252,#12253,#12254,#12255,#12256,
#12257,#12258,#12259,#12260,#12261,#12262,#12263),.UNSPECIFIED.,.F.,.F.,
(4,2,2,2,2,4),(0.373895639787233,0.434492857144191,0.495090074501149,0.558265375769478,
0.621440677037807,0.7004435143378),.UNSPECIFIED.);
#289=B_SPLINE_CURVE_WITH_KNOTS('',3,(#12270,#12271,#12272,#12273,#12274,
#12275,#12276,#12277,#12278,#12279,#12280,#12281,#12282,#12283,#12284,#12285,
#12286,#12287,#12288,#12289,#12290,#12291),.UNSPECIFIED.,.F.,.F.,(4,2,2,
2,2,2,2,2,2,2,4),(0.0473477652366656,0.126350602536658,0.189525903804987,
0.252701205073316,0.313298422430275,0.373895639787233,0.434492857144191,
0.495090074501149,0.558265375769478,0.621440677037807,0.7004435143378),
 .UNSPECIFIED.);
#290=B_SPLINE_CURVE_WITH_KNOTS('',3,(#12299,#12300,#12301,#12302,#12303,
#12304,#12305,#12306,#12307,#12308,#12309,#12310,#12311,#12312,#12313,#12314,
#12315,#12316,#12317,#12318,#12319,#12320),.UNSPECIFIED.,.F.,.F.,(4,2,2,
2,2,2,2,2,2,2,4),(0.0473477652366656,0.126350602536658,0.189525903804987,
0.252701205073317,0.313298422430275,0.373895639787233,0.434492857144191,
0.495090074501149,0.558265375769478,0.621440677037807,0.7004435143378),
 .UNSPECIFIED.);
#291=B_SPLINE_CURVE_WITH_KNOTS('',3,(#12328,#12329,#12330,#12331,#12332,
#12333,#12334,#12335,#12336,#12337,#12338,#12339,#12340,#12341,#12342,#12343,
#12344,#12345,#12346,#12347,#12348,#12349),.UNSPECIFIED.,.F.,.F.,(4,2,2,
2,2,2,2,2,2,2,4),(0.0473477652366656,0.126350602536658,0.189525903804987,
0.252701205073316,0.313298422430275,0.373895639787233,0.434492857144191,
0.495090074501149,0.558265375769478,0.621440677037807,0.7004435143378),
 .UNSPECIFIED.);
#292=B_SPLINE_CURVE_WITH_KNOTS('',3,(#12358,#12359,#12360,#12361,#12362,
#12363,#12364,#12365,#12366,#12367,#12368,#12369,#12370,#12371,#12372,#12373,
#12374,#12375,#12376,#12377,#12378,#12379),.UNSPECIFIED.,.F.,.F.,(4,2,2,
2,2,2,2,2,2,2,4),(0.0473477652366656,0.126350602536658,0.189525903804987,
0.252701205073317,0.313298422430275,0.373895639787233,0.434492857144191,
0.495090074501149,0.558265375769478,0.621440677037807,0.7004435143378),
 .UNSPECIFIED.);
#293=SPHERICAL_SURFACE('',#7199,0.3969);
#294=SPHERICAL_SURFACE('',#7201,0.3969);
#295=SPHERICAL_SURFACE('',#7203,0.3969);
#296=SPHERICAL_SURFACE('',#7205,0.3969);
#297=SPHERICAL_SURFACE('',#7207,0.3969);
#298=SPHERICAL_SURFACE('',#7209,0.3969);
#299=SPHERICAL_SURFACE('',#7211,0.3969);
#300=SPHERICAL_SURFACE('',#7213,0.3969);
#301=SPHERICAL_SURFACE('',#7215,0.3969);
#302=SPHERICAL_SURFACE('',#7218,0.412776);
#303=SPHERICAL_SURFACE('',#7236,0.412776);
#304=SPHERICAL_SURFACE('',#7241,0.412776);
#305=SPHERICAL_SURFACE('',#7246,0.412776);
#306=SPHERICAL_SURFACE('',#7252,0.412776);
#307=SPHERICAL_SURFACE('',#7257,0.412776);
#308=SPHERICAL_SURFACE('',#7262,0.412776);
#309=SPHERICAL_SURFACE('',#7267,0.412776);
#310=SPHERICAL_SURFACE('',#7275,0.412776);
#311=SPHERICAL_SURFACE('',#7579,0.23815);
#312=SPHERICAL_SURFACE('',#7581,0.23815);
#313=SPHERICAL_SURFACE('',#7583,0.23815);
#314=SPHERICAL_SURFACE('',#7585,0.23815);
#315=SPHERICAL_SURFACE('',#7587,0.23815);
#316=SPHERICAL_SURFACE('',#7589,0.23815);
#317=SPHERICAL_SURFACE('',#7591,0.23815);
#318=SPHERICAL_SURFACE('',#7593,0.23815);
#319=SPHERICAL_SURFACE('',#7596,0.247676);
#320=SPHERICAL_SURFACE('',#7612,0.247676);
#321=SPHERICAL_SURFACE('',#7617,0.247676);
#322=SPHERICAL_SURFACE('',#7622,0.247676);
#323=SPHERICAL_SURFACE('',#7627,0.247676);
#324=SPHERICAL_SURFACE('',#7632,0.247676);
#325=SPHERICAL_SURFACE('',#7637,0.247676);
#326=SPHERICAL_SURFACE('',#7645,0.247676);
#327=CONICAL_SURFACE('',#7170,1.3,0.785398163397449);
#328=CONICAL_SURFACE('',#7177,1.3,0.785398163397449);
#329=CONICAL_SURFACE('',#7190,2.55,0.785398163397449);
#330=CONICAL_SURFACE('',#7194,2.55,0.785398163397449);
#331=CONICAL_SURFACE('',#7304,0.475,0.785398163397449);
#332=CONICAL_SURFACE('',#7308,0.485,0.785398163397448);
#333=CONICAL_SURFACE('',#7312,0.31,0.463647609000806);
#334=CONICAL_SURFACE('',#7316,0.27,0.785398163397448);
#335=CONICAL_SURFACE('',#7330,0.325,0.785398163397448);
#336=CONICAL_SURFACE('',#7334,0.335,0.785398163397448);
#337=CONICAL_SURFACE('',#7338,0.21,0.463647609000806);
#338=CONICAL_SURFACE('',#7342,0.18,0.785398163397448);
#339=CONICAL_SURFACE('',#7530,0.235,0.785398163397448);
#340=CONICAL_SURFACE('',#7534,0.2125,0.785398163397448);
#341=CONICAL_SURFACE('',#7550,0.53,0.785398163397448);
#342=CONICAL_SURFACE('',#7557,0.53,0.785398163397448);
#343=CONICAL_SURFACE('',#7570,1.47,0.785398163397449);
#344=CONICAL_SURFACE('',#7574,1.47,0.785398163397449);
#345=CONICAL_SURFACE('',#7786,0.325,0.785398163397448);
#346=CONICAL_SURFACE('',#7790,0.335,0.785398163397448);
#347=CONICAL_SURFACE('',#7794,0.21,0.463647609000806);
#348=TOROIDAL_SURFACE('',#7159,1.925,0.412776);
#349=TOROIDAL_SURFACE('',#7179,1.925,0.412776);
#350=TOROIDAL_SURFACE('',#7539,1.,0.247676);
#351=TOROIDAL_SURFACE('',#7559,1.,0.247676);
#352=SHAPE_REPRESENTATION_RELATIONSHIP('SRR','None',#12933,#389);
#353=SHAPE_REPRESENTATION_RELATIONSHIP('SRR','None',#12934,#390);
#354=SHAPE_REPRESENTATION_RELATIONSHIP('SRR','None',#12935,#391);
#355=SHAPE_REPRESENTATION_RELATIONSHIP('SRR','None',#12936,#392);
#356=SHAPE_REPRESENTATION_RELATIONSHIP('SRR','None',#12937,#393);
#357=SHAPE_REPRESENTATION_RELATIONSHIP('SRR','None',#12938,#394);
#358=SHAPE_REPRESENTATION_RELATIONSHIP('SRR','None',#12939,#395);
#359=SHAPE_REPRESENTATION_RELATIONSHIP('SRR','None',#12941,#396);
#360=SHAPE_REPRESENTATION_RELATIONSHIP('SRR','None',#12942,#397);
#361=SHAPE_REPRESENTATION_RELATIONSHIP('SRR','None',#12943,#398);
#362=SHAPE_REPRESENTATION_RELATIONSHIP('SRR','None',#12944,#399);
#363=SHAPE_REPRESENTATION_RELATIONSHIP('SRR','None',#12945,#400);
#364=SHAPE_REPRESENTATION_RELATIONSHIP('SRR','None',#12946,#401);
#365=SHAPE_REPRESENTATION_RELATIONSHIP('SRR','None',#12947,#402);
#366=SHAPE_REPRESENTATION_RELATIONSHIP('SRR','None',#12949,#403);
#367=SHAPE_REPRESENTATION_RELATIONSHIP('SRR','None',#12950,#404);
#368=SHAPE_REPRESENTATION_RELATIONSHIP('SRR','None',#12951,#405);
#369=SHAPE_REPRESENTATION_RELATIONSHIP('SRR','None',#12952,#406);
#370=SHAPE_REPRESENTATION_RELATIONSHIP('SRR','None',#12953,#407);
#371=SHAPE_REPRESENTATION_RELATIONSHIP('SRR','None',#12954,#408);
#372=SHAPE_REPRESENTATION_RELATIONSHIP('SRR','None',#12955,#409);
#373=SHAPE_REPRESENTATION_RELATIONSHIP('SRR','None',#12956,#410);
#374=SHAPE_REPRESENTATION_RELATIONSHIP('SRR','None',#12957,#411);
#375=SHAPE_REPRESENTATION_RELATIONSHIP('SRR','None',#12959,#412);
#376=SHAPE_REPRESENTATION_RELATIONSHIP('SRR','None',#12960,#413);
#377=SHAPE_REPRESENTATION_RELATIONSHIP('SRR','None',#12961,#414);
#378=SHAPE_REPRESENTATION_RELATIONSHIP('SRR','None',#12962,#415);
#379=SHAPE_REPRESENTATION_RELATIONSHIP('SRR','None',#12963,#416);
#380=SHAPE_REPRESENTATION_RELATIONSHIP('SRR','None',#12965,#417);
#381=SHAPE_REPRESENTATION_RELATIONSHIP('SRR','None',#12966,#418);
#382=SHAPE_REPRESENTATION_RELATIONSHIP('SRR','None',#12967,#419);
#383=SHAPE_REPRESENTATION_RELATIONSHIP('SRR','None',#12968,#420);
#384=SHAPE_REPRESENTATION_RELATIONSHIP('SRR','None',#12969,#421);
#385=SHAPE_REPRESENTATION_RELATIONSHIP('SRR','None',#12970,#422);
#386=SHAPE_REPRESENTATION_RELATIONSHIP('SRR','None',#12971,#423);
#387=SHAPE_REPRESENTATION_RELATIONSHIP('SRR','None',#12972,#424);
#388=SHAPE_REPRESENTATION_RELATIONSHIP('SRR','None',#12973,#425);
#389=ADVANCED_BREP_SHAPE_REPRESENTATION('',(#480),#12742);
#390=ADVANCED_BREP_SHAPE_REPRESENTATION('',(#481),#12743);
#391=ADVANCED_BREP_SHAPE_REPRESENTATION('',(#482),#12744);
#392=ADVANCED_BREP_SHAPE_REPRESENTATION('',(#483),#12745);
#393=ADVANCED_BREP_SHAPE_REPRESENTATION('',(#484),#12746);
#394=ADVANCED_BREP_SHAPE_REPRESENTATION('',(#485),#12747);
#395=ADVANCED_BREP_SHAPE_REPRESENTATION('',(#486),#12748);
#396=ADVANCED_BREP_SHAPE_REPRESENTATION('',(#487),#12750);
#397=ADVANCED_BREP_SHAPE_REPRESENTATION('',(#488),#12751);
#398=ADVANCED_BREP_SHAPE_REPRESENTATION('',(#489,#490,#491,#492,#493,#494,
#495,#496,#497),#12752);
#399=ADVANCED_BREP_SHAPE_REPRESENTATION('',(#498),#12753);
#400=ADVANCED_BREP_SHAPE_REPRESENTATION('',(#499,#500),#12754);
#401=ADVANCED_BREP_SHAPE_REPRESENTATION('',(#14),#12755);
#402=ADVANCED_BREP_SHAPE_REPRESENTATION('',(#15),#12756);
#403=ADVANCED_BREP_SHAPE_REPRESENTATION('',(#501),#12758);
#404=ADVANCED_BREP_SHAPE_REPRESENTATION('',(#502),#12759);
#405=ADVANCED_BREP_SHAPE_REPRESENTATION('',(#503),#12760);
#406=ADVANCED_BREP_SHAPE_REPRESENTATION('',(#504),#12761);
#407=ADVANCED_BREP_SHAPE_REPRESENTATION('',(#505),#12762);
#408=ADVANCED_BREP_SHAPE_REPRESENTATION('',(#506),#12763);
#409=ADVANCED_BREP_SHAPE_REPRESENTATION('',(#507),#12764);
#410=ADVANCED_BREP_SHAPE_REPRESENTATION('',(#508),#12765);
#411=ADVANCED_BREP_SHAPE_REPRESENTATION('',(#509),#12766);
#412=ADVANCED_BREP_SHAPE_REPRESENTATION('',(#510),#12768);
#413=ADVANCED_BREP_SHAPE_REPRESENTATION('',(#511),#12769);
#414=ADVANCED_BREP_SHAPE_REPRESENTATION('',(#512,#513,#514,#515,#516,#517,
#518,#519),#12770);
#415=ADVANCED_BREP_SHAPE_REPRESENTATION('',(#520),#12771);
#416=ADVANCED_BREP_SHAPE_REPRESENTATION('',(#521,#522),#12772);
#417=ADVANCED_BREP_SHAPE_REPRESENTATION('',(#523),#12774);
#418=ADVANCED_BREP_SHAPE_REPRESENTATION('',(#524),#12775);
#419=ADVANCED_BREP_SHAPE_REPRESENTATION('',(#525),#12776);
#420=ADVANCED_BREP_SHAPE_REPRESENTATION('',(#526),#12777);
#421=ADVANCED_BREP_SHAPE_REPRESENTATION('',(#527),#12778);
#422=ADVANCED_BREP_SHAPE_REPRESENTATION('',(#528),#12779);
#423=ADVANCED_BREP_SHAPE_REPRESENTATION('',(#529),#12780);
#424=ADVANCED_BREP_SHAPE_REPRESENTATION('',(#530),#12781);
#425=ADVANCED_BREP_SHAPE_REPRESENTATION('',(#16),#12782);
#426=STYLED_ITEM('',(#13191),#480);
#427=STYLED_ITEM('',(#13212),#481);
#428=STYLED_ITEM('',(#13212),#482);
#429=STYLED_ITEM('',(#13212),#483);
#430=STYLED_ITEM('',(#13212),#484);
#431=STYLED_ITEM('',(#13226),#485);
#432=STYLED_ITEM('',(#13226),#486);
#433=STYLED_ITEM('',(#13212),#487);
#434=STYLED_ITEM('',(#13212),#488);
#435=STYLED_ITEM('',(#13212),#489);
#436=STYLED_ITEM('',(#13212),#490);
#437=STYLED_ITEM('',(#13212),#491);
#438=STYLED_ITEM('',(#13212),#492);
#439=STYLED_ITEM('',(#13212),#493);
#440=STYLED_ITEM('',(#13212),#494);
#441=STYLED_ITEM('',(#13212),#495);
#442=STYLED_ITEM('',(#13212),#496);
#443=STYLED_ITEM('',(#13212),#497);
#444=STYLED_ITEM('',(#13212),#498);
#445=STYLED_ITEM('',(#13212),#499);
#446=STYLED_ITEM('',(#13212),#500);
#447=STYLED_ITEM('',(#13219),#14);
#448=STYLED_ITEM('',(#13219),#15);
#449=STYLED_ITEM('',(#13212),#501);
#450=STYLED_ITEM('',(#13212),#502);
#451=STYLED_ITEM('',(#13212),#503);
#452=STYLED_ITEM('',(#13198),#504);
#453=STYLED_ITEM('',(#13205),#505);
#454=STYLED_ITEM('',(#13212),#506);
#455=STYLED_ITEM('',(#13212),#507);
#456=STYLED_ITEM('',(#13212),#508);
#457=STYLED_ITEM('',(#13219),#509);
#458=STYLED_ITEM('',(#13212),#510);
#459=STYLED_ITEM('',(#13212),#511);
#460=STYLED_ITEM('',(#13212),#512);
#461=STYLED_ITEM('',(#13212),#513);
#462=STYLED_ITEM('',(#13212),#514);
#463=STYLED_ITEM('',(#13212),#515);
#464=STYLED_ITEM('',(#13212),#516);
#465=STYLED_ITEM('',(#13212),#517);
#466=STYLED_ITEM('',(#13212),#518);
#467=STYLED_ITEM('',(#13212),#519);
#468=STYLED_ITEM('',(#13212),#520);
#469=STYLED_ITEM('',(#13212),#521);
#470=STYLED_ITEM('',(#13212),#522);
#471=STYLED_ITEM('',(#13198),#523);
#472=STYLED_ITEM('',(#13212),#524);
#473=STYLED_ITEM('',(#13205),#525);
#474=STYLED_ITEM('',(#13205),#526);
#475=STYLED_ITEM('',(#13205),#527);
#476=STYLED_ITEM('',(#13205),#528);
#477=STYLED_ITEM('',(#13205),#529);
#478=STYLED_ITEM('',(#13205),#530);
#479=STYLED_ITEM('',(#13219),#16);
#480=MANIFOLD_SOLID_BREP('Body1',#6495);
#481=MANIFOLD_SOLID_BREP('Body1',#6496);
#482=MANIFOLD_SOLID_BREP('Body1',#6497);
#483=MANIFOLD_SOLID_BREP('Body1',#6498);
#484=MANIFOLD_SOLID_BREP('Body1',#6499);
#485=MANIFOLD_SOLID_BREP('Body1',#6500);
#486=MANIFOLD_SOLID_BREP('Body1',#6501);
#487=MANIFOLD_SOLID_BREP('Body1',#6502);
#488=MANIFOLD_SOLID_BREP('Body1',#6503);
#489=MANIFOLD_SOLID_BREP('Body1',#6504);
#490=MANIFOLD_SOLID_BREP('Body2',#6505);
#491=MANIFOLD_SOLID_BREP('Body3',#6506);
#492=MANIFOLD_SOLID_BREP('Body4',#6507);
#493=MANIFOLD_SOLID_BREP('Body5',#6508);
#494=MANIFOLD_SOLID_BREP('Body6',#6509);
#495=MANIFOLD_SOLID_BREP('Body7',#6510);
#496=MANIFOLD_SOLID_BREP('Body8',#6511);
#497=MANIFOLD_SOLID_BREP('Body9',#6512);
#498=MANIFOLD_SOLID_BREP('Continuous crown cage',#6513);
#499=MANIFOLD_SOLID_BREP('Body1',#6514);
#500=MANIFOLD_SOLID_BREP('Body2',#6515);
#501=MANIFOLD_SOLID_BREP('Body1',#6520);
#502=MANIFOLD_SOLID_BREP('Body1',#6521);
#503=MANIFOLD_SOLID_BREP('Body1',#6522);
#504=MANIFOLD_SOLID_BREP('Body1',#6523);
#505=MANIFOLD_SOLID_BREP('Body1',#6524);
#506=MANIFOLD_SOLID_BREP('Body1',#6525);
#507=MANIFOLD_SOLID_BREP('Body1',#6526);
#508=MANIFOLD_SOLID_BREP('Body1',#6527);
#509=MANIFOLD_SOLID_BREP('Body1',#6528);
#510=MANIFOLD_SOLID_BREP('Body1',#6529);
#511=MANIFOLD_SOLID_BREP('Body1',#6530);
#512=MANIFOLD_SOLID_BREP('Body1',#6531);
#513=MANIFOLD_SOLID_BREP('Body2',#6532);
#514=MANIFOLD_SOLID_BREP('Body3',#6533);
#515=MANIFOLD_SOLID_BREP('Body4',#6534);
#516=MANIFOLD_SOLID_BREP('Body5',#6535);
#517=MANIFOLD_SOLID_BREP('Body6',#6536);
#518=MANIFOLD_SOLID_BREP('Body7',#6537);
#519=MANIFOLD_SOLID_BREP('Body8',#6538);
#520=MANIFOLD_SOLID_BREP('Continuous crown cage',#6539);
#521=MANIFOLD_SOLID_BREP('Body1',#6540);
#522=MANIFOLD_SOLID_BREP('Body2',#6541);
#523=MANIFOLD_SOLID_BREP('Body1',#6542);
#524=MANIFOLD_SOLID_BREP('Body1',#6543);
#525=MANIFOLD_SOLID_BREP('Body1',#6544);
#526=MANIFOLD_SOLID_BREP('Body1',#6545);
#527=MANIFOLD_SOLID_BREP('Body1',#6546);
#528=MANIFOLD_SOLID_BREP('Body1',#6547);
#529=MANIFOLD_SOLID_BREP('Body1',#6548);
#530=MANIFOLD_SOLID_BREP('Body1',#6549);
#531=FACE_BOUND('',#1279,.T.);
#532=FACE_BOUND('',#1280,.T.);
#533=FACE_BOUND('',#1281,.T.);
#534=FACE_BOUND('',#1282,.T.);
#535=FACE_BOUND('',#1284,.T.);
#536=FACE_BOUND('',#1285,.T.);
#537=FACE_BOUND('',#1286,.T.);
#538=FACE_BOUND('',#1287,.T.);
#539=FACE_BOUND('',#1307,.T.);
#540=FACE_BOUND('',#1311,.T.);
#541=FACE_BOUND('',#1315,.T.);
#542=FACE_BOUND('',#1319,.T.);
#543=FACE_BOUND('',#1336,.T.);
#544=FACE_BOUND('',#1337,.T.);
#545=FACE_BOUND('',#1342,.T.);
#546=FACE_BOUND('',#1343,.T.);
#547=FACE_BOUND('',#1348,.T.);
#548=FACE_BOUND('',#1349,.T.);
#549=FACE_BOUND('',#1351,.T.);
#550=FACE_BOUND('',#1352,.T.);
#551=FACE_BOUND('',#1353,.T.);
#552=FACE_BOUND('',#1354,.T.);
#553=FACE_BOUND('',#1355,.T.);
#554=FACE_BOUND('',#1357,.T.);
#555=FACE_BOUND('',#1358,.T.);
#556=FACE_BOUND('',#1359,.T.);
#557=FACE_BOUND('',#1360,.T.);
#558=FACE_BOUND('',#1361,.T.);
#559=FACE_BOUND('',#1365,.T.);
#560=FACE_BOUND('',#1367,.T.);
#561=FACE_BOUND('',#1374,.T.);
#562=FACE_BOUND('',#1378,.T.);
#563=FACE_BOUND('',#1379,.T.);
#564=FACE_BOUND('',#1380,.T.);
#565=FACE_BOUND('',#1381,.T.);
#566=FACE_BOUND('',#1382,.T.);
#567=FACE_BOUND('',#1384,.T.);
#568=FACE_BOUND('',#1385,.T.);
#569=FACE_BOUND('',#1386,.T.);
#570=FACE_BOUND('',#1387,.T.);
#571=FACE_BOUND('',#1388,.T.);
#572=FACE_BOUND('',#1395,.T.);
#573=FACE_BOUND('',#1399,.T.);
#574=FACE_BOUND('',#1400,.T.);
#575=FACE_BOUND('',#1401,.T.);
#576=FACE_BOUND('',#1402,.T.);
#577=FACE_BOUND('',#1403,.T.);
#578=FACE_BOUND('',#1405,.T.);
#579=FACE_BOUND('',#1406,.T.);
#580=FACE_BOUND('',#1407,.T.);
#581=FACE_BOUND('',#1408,.T.);
#582=FACE_BOUND('',#1409,.T.);
#583=FACE_BOUND('',#1427,.T.);
#584=FACE_BOUND('',#1430,.T.);
#585=FACE_BOUND('',#1435,.T.);
#586=FACE_BOUND('',#1440,.T.);
#587=FACE_BOUND('',#1471,.T.);
#588=FACE_BOUND('',#1474,.T.);
#589=FACE_BOUND('',#1477,.T.);
#590=FACE_BOUND('',#1480,.T.);
#591=FACE_BOUND('',#1483,.T.);
#592=FACE_BOUND('',#1490,.T.);
#593=FACE_BOUND('',#1508,.T.);
#594=FACE_BOUND('',#1532,.T.);
#595=FACE_BOUND('',#1534,.T.);
#596=FACE_BOUND('',#1537,.T.);
#597=FACE_BOUND('',#1539,.T.);
#598=FACE_BOUND('',#1545,.T.);
#599=FACE_BOUND('',#1547,.T.);
#600=FACE_BOUND('',#1552,.T.);
#601=FACE_BOUND('',#1554,.T.);
#602=FACE_BOUND('',#1556,.T.);
#603=FACE_BOUND('',#1558,.T.);
#604=FACE_BOUND('',#1568,.T.);
#605=FACE_BOUND('',#1576,.T.);
#606=FACE_BOUND('',#1578,.T.);
#607=FACE_BOUND('',#1580,.T.);
#608=FACE_BOUND('',#1588,.T.);
#609=FACE_BOUND('',#1590,.T.);
#610=FACE_BOUND('',#1594,.T.);
#611=FACE_BOUND('',#1597,.T.);
#612=FACE_BOUND('',#1600,.T.);
#613=FACE_BOUND('',#1601,.T.);
#614=FACE_BOUND('',#1603,.T.);
#615=FACE_BOUND('',#1606,.T.);
#616=FACE_BOUND('',#1610,.T.);
#617=FACE_BOUND('',#1612,.T.);
#618=FACE_BOUND('',#1615,.T.);
#619=FACE_BOUND('',#1619,.T.);
#620=FACE_BOUND('',#1621,.T.);
#621=FACE_BOUND('',#1640,.T.);
#622=FACE_BOUND('',#1650,.T.);
#623=FACE_BOUND('',#1653,.T.);
#624=FACE_BOUND('',#1658,.T.);
#625=FACE_BOUND('',#1663,.T.);
#626=FACE_BOUND('',#1691,.T.);
#627=FACE_BOUND('',#1694,.T.);
#628=FACE_BOUND('',#1697,.T.);
#629=FACE_BOUND('',#1700,.T.);
#630=FACE_BOUND('',#1703,.T.);
#631=FACE_BOUND('',#1709,.T.);
#632=FACE_BOUND('',#1712,.T.);
#633=FACE_BOUND('',#1714,.T.);
#634=FACE_BOUND('',#1716,.T.);
#635=FACE_BOUND('',#1719,.T.);
#636=FACE_BOUND('',#1723,.T.);
#637=FACE_BOUND('',#1730,.T.);
#638=FACE_BOUND('',#1732,.T.);
#639=FACE_BOUND('',#1736,.T.);
#640=FACE_BOUND('',#1738,.T.);
#641=FACE_BOUND('',#1742,.T.);
#642=FACE_BOUND('',#1744,.T.);
#643=FACE_BOUND('',#1748,.T.);
#644=FACE_BOUND('',#1750,.T.);
#645=FACE_BOUND('',#1754,.T.);
#646=FACE_BOUND('',#1756,.T.);
#647=FACE_BOUND('',#1760,.T.);
#648=FACE_BOUND('',#1762,.T.);
#649=FACE_BOUND('',#1766,.T.);
#650=FACE_BOUND('',#1768,.T.);
#651=FACE_BOUND('',#1783,.T.);
#652=PLANE('',#6975);
#653=PLANE('',#6976);
#654=PLANE('',#6977);
#655=PLANE('',#6978);
#656=PLANE('',#6979);
#657=PLANE('',#6980);
#658=PLANE('',#6985);
#659=PLANE('',#6989);
#660=PLANE('',#6993);
#661=PLANE('',#6997);
#662=PLANE('',#7001);
#663=PLANE('',#7005);
#664=PLANE('',#7009);
#665=PLANE('',#7013);
#666=PLANE('',#7020);
#667=PLANE('',#7028);
#668=PLANE('',#7036);
#669=PLANE('',#7044);
#670=PLANE('',#7046);
#671=PLANE('',#7047);
#672=PLANE('',#7048);
#673=PLANE('',#7049);
#674=PLANE('',#7050);
#675=PLANE('',#7052);
#676=PLANE('',#7053);
#677=PLANE('',#7054);
#678=PLANE('',#7056);
#679=PLANE('',#7057);
#680=PLANE('',#7066);
#681=PLANE('',#7067);
#682=PLANE('',#7068);
#683=PLANE('',#7069);
#684=PLANE('',#7071);
#685=PLANE('',#7072);
#686=PLANE('',#7073);
#687=PLANE('',#7074);
#688=PLANE('',#7082);
#689=PLANE('',#7083);
#690=PLANE('',#7091);
#691=PLANE('',#7092);
#692=PLANE('',#7109);
#693=PLANE('',#7116);
#694=PLANE('',#7117);
#695=PLANE('',#7134);
#696=PLANE('',#7141);
#697=PLANE('',#7142);
#698=PLANE('',#7144);
#699=PLANE('',#7145);
#700=PLANE('',#7146);
#701=PLANE('',#7147);
#702=PLANE('',#7148);
#703=PLANE('',#7149);
#704=PLANE('',#7151);
#705=PLANE('',#7152);
#706=PLANE('',#7153);
#707=PLANE('',#7154);
#708=PLANE('',#7155);
#709=PLANE('',#7156);
#710=PLANE('',#7172);
#711=PLANE('',#7175);
#712=PLANE('',#7187);
#713=PLANE('',#7196);
#714=PLANE('',#7233);
#715=PLANE('',#7238);
#716=PLANE('',#7243);
#717=PLANE('',#7248);
#718=PLANE('',#7254);
#719=PLANE('',#7259);
#720=PLANE('',#7264);
#721=PLANE('',#7273);
#722=PLANE('',#7277);
#723=PLANE('',#7278);
#724=PLANE('',#7280);
#725=PLANE('',#7285);
#726=PLANE('',#7288);
#727=PLANE('',#7293);
#728=PLANE('',#7302);
#729=PLANE('',#7310);
#730=PLANE('',#7318);
#731=PLANE('',#7319);
#732=PLANE('',#7320);
#733=PLANE('',#7321);
#734=PLANE('',#7322);
#735=PLANE('',#7323);
#736=PLANE('',#7324);
#737=PLANE('',#7325);
#738=PLANE('',#7326);
#739=PLANE('',#7328);
#740=PLANE('',#7336);
#741=PLANE('',#7344);
#742=PLANE('',#7345);
#743=PLANE('',#7346);
#744=PLANE('',#7347);
#745=PLANE('',#7348);
#746=PLANE('',#7349);
#747=PLANE('',#7350);
#748=PLANE('',#7351);
#749=PLANE('',#7352);
#750=PLANE('',#7376);
#751=PLANE('',#7377);
#752=PLANE('',#7379);
#753=PLANE('',#7380);
#754=PLANE('',#7381);
#755=PLANE('',#7383);
#756=PLANE('',#7384);
#757=PLANE('',#7386);
#758=PLANE('',#7387);
#759=PLANE('',#7388);
#760=PLANE('',#7390);
#761=PLANE('',#7393);
#762=PLANE('',#7401);
#763=PLANE('',#7402);
#764=PLANE('',#7410);
#765=PLANE('',#7411);
#766=PLANE('',#7413);
#767=PLANE('',#7418);
#768=PLANE('',#7425);
#769=PLANE('',#7426);
#770=PLANE('',#7428);
#771=PLANE('',#7433);
#772=PLANE('',#7434);
#773=PLANE('',#7435);
#774=PLANE('',#7436);
#775=PLANE('',#7437);
#776=PLANE('',#7438);
#777=PLANE('',#7439);
#778=PLANE('',#7442);
#779=PLANE('',#7443);
#780=PLANE('',#7444);
#781=PLANE('',#7445);
#782=PLANE('',#7446);
#783=PLANE('',#7447);
#784=PLANE('',#7449);
#785=PLANE('',#7454);
#786=PLANE('',#7459);
#787=PLANE('',#7460);
#788=PLANE('',#7461);
#789=PLANE('',#7462);
#790=PLANE('',#7463);
#791=PLANE('',#7474);
#792=PLANE('',#7476);
#793=PLANE('',#7477);
#794=PLANE('',#7479);
#795=PLANE('',#7482);
#796=PLANE('',#7487);
#797=PLANE('',#7494);
#798=PLANE('',#7495);
#799=PLANE('',#7500);
#800=PLANE('',#7507);
#801=PLANE('',#7508);
#802=PLANE('',#7510);
#803=PLANE('',#7511);
#804=PLANE('',#7512);
#805=PLANE('',#7513);
#806=PLANE('',#7514);
#807=PLANE('',#7515);
#808=PLANE('',#7516);
#809=PLANE('',#7517);
#810=PLANE('',#7518);
#811=PLANE('',#7519);
#812=PLANE('',#7521);
#813=PLANE('',#7522);
#814=PLANE('',#7523);
#815=PLANE('',#7524);
#816=PLANE('',#7525);
#817=PLANE('',#7526);
#818=PLANE('',#7527);
#819=PLANE('',#7528);
#820=PLANE('',#7536);
#821=PLANE('',#7552);
#822=PLANE('',#7555);
#823=PLANE('',#7567);
#824=PLANE('',#7576);
#825=PLANE('',#7609);
#826=PLANE('',#7614);
#827=PLANE('',#7619);
#828=PLANE('',#7624);
#829=PLANE('',#7629);
#830=PLANE('',#7634);
#831=PLANE('',#7643);
#832=PLANE('',#7647);
#833=PLANE('',#7648);
#834=PLANE('',#7650);
#835=PLANE('',#7655);
#836=PLANE('',#7658);
#837=PLANE('',#7663);
#838=PLANE('',#7695);
#839=PLANE('',#7696);
#840=PLANE('',#7697);
#841=PLANE('',#7698);
#842=PLANE('',#7699);
#843=PLANE('',#7700);
#844=PLANE('',#7701);
#845=PLANE('',#7702);
#846=PLANE('',#7703);
#847=PLANE('',#7704);
#848=PLANE('',#7709);
#849=PLANE('',#7713);
#850=PLANE('',#7717);
#851=PLANE('',#7718);
#852=PLANE('',#7726);
#853=PLANE('',#7727);
#854=PLANE('',#7735);
#855=PLANE('',#7736);
#856=PLANE('',#7744);
#857=PLANE('',#7745);
#858=PLANE('',#7753);
#859=PLANE('',#7754);
#860=PLANE('',#7762);
#861=PLANE('',#7763);
#862=PLANE('',#7771);
#863=PLANE('',#7772);
#864=PLANE('',#7774);
#865=PLANE('',#7775);
#866=PLANE('',#7776);
#867=PLANE('',#7777);
#868=PLANE('',#7778);
#869=PLANE('',#7779);
#870=PLANE('',#7780);
#871=PLANE('',#7781);
#872=PLANE('',#7782);
#873=PLANE('',#7784);
#874=PLANE('',#7792);
#875=FACE_OUTER_BOUND('',#1270,.T.);
#876=FACE_OUTER_BOUND('',#1271,.T.);
#877=FACE_OUTER_BOUND('',#1272,.T.);
#878=FACE_OUTER_BOUND('',#1273,.T.);
#879=FACE_OUTER_BOUND('',#1274,.T.);
#880=FACE_OUTER_BOUND('',#1275,.T.);
#881=FACE_OUTER_BOUND('',#1276,.T.);
#882=FACE_OUTER_BOUND('',#1277,.T.);
#883=FACE_OUTER_BOUND('',#1278,.T.);
#884=FACE_OUTER_BOUND('',#1283,.T.);
#885=FACE_OUTER_BOUND('',#1288,.T.);
#886=FACE_OUTER_BOUND('',#1289,.T.);
#887=FACE_OUTER_BOUND('',#1290,.T.);
#888=FACE_OUTER_BOUND('',#1291,.T.);
#889=FACE_OUTER_BOUND('',#1292,.T.);
#890=FACE_OUTER_BOUND('',#1293,.T.);
#891=FACE_OUTER_BOUND('',#1294,.T.);
#892=FACE_OUTER_BOUND('',#1295,.T.);
#893=FACE_OUTER_BOUND('',#1296,.T.);
#894=FACE_OUTER_BOUND('',#1297,.T.);
#895=FACE_OUTER_BOUND('',#1298,.T.);
#896=FACE_OUTER_BOUND('',#1299,.T.);
#897=FACE_OUTER_BOUND('',#1300,.T.);
#898=FACE_OUTER_BOUND('',#1301,.T.);
#899=FACE_OUTER_BOUND('',#1302,.T.);
#900=FACE_OUTER_BOUND('',#1303,.T.);
#901=FACE_OUTER_BOUND('',#1304,.T.);
#902=FACE_OUTER_BOUND('',#1305,.T.);
#903=FACE_OUTER_BOUND('',#1306,.T.);
#904=FACE_OUTER_BOUND('',#1308,.T.);
#905=FACE_OUTER_BOUND('',#1309,.T.);
#906=FACE_OUTER_BOUND('',#1310,.T.);
#907=FACE_OUTER_BOUND('',#1312,.T.);
#908=FACE_OUTER_BOUND('',#1313,.T.);
#909=FACE_OUTER_BOUND('',#1314,.T.);
#910=FACE_OUTER_BOUND('',#1316,.T.);
#911=FACE_OUTER_BOUND('',#1317,.T.);
#912=FACE_OUTER_BOUND('',#1318,.T.);
#913=FACE_OUTER_BOUND('',#1320,.T.);
#914=FACE_OUTER_BOUND('',#1321,.T.);
#915=FACE_OUTER_BOUND('',#1322,.T.);
#916=FACE_OUTER_BOUND('',#1323,.T.);
#917=FACE_OUTER_BOUND('',#1324,.T.);
#918=FACE_OUTER_BOUND('',#1325,.T.);
#919=FACE_OUTER_BOUND('',#1326,.T.);
#920=FACE_OUTER_BOUND('',#1327,.T.);
#921=FACE_OUTER_BOUND('',#1328,.T.);
#922=FACE_OUTER_BOUND('',#1329,.T.);
#923=FACE_OUTER_BOUND('',#1330,.T.);
#924=FACE_OUTER_BOUND('',#1331,.T.);
#925=FACE_OUTER_BOUND('',#1332,.T.);
#926=FACE_OUTER_BOUND('',#1333,.T.);
#927=FACE_OUTER_BOUND('',#1334,.T.);
#928=FACE_OUTER_BOUND('',#1335,.T.);
#929=FACE_OUTER_BOUND('',#1338,.T.);
#930=FACE_OUTER_BOUND('',#1339,.T.);
#931=FACE_OUTER_BOUND('',#1340,.T.);
#932=FACE_OUTER_BOUND('',#1341,.T.);
#933=FACE_OUTER_BOUND('',#1344,.T.);
#934=FACE_OUTER_BOUND('',#1345,.T.);
#935=FACE_OUTER_BOUND('',#1346,.T.);
#936=FACE_OUTER_BOUND('',#1347,.T.);
#937=FACE_OUTER_BOUND('',#1350,.T.);
#938=FACE_OUTER_BOUND('',#1356,.T.);
#939=FACE_OUTER_BOUND('',#1362,.T.);
#940=FACE_OUTER_BOUND('',#1363,.T.);
#941=FACE_OUTER_BOUND('',#1364,.T.);
#942=FACE_OUTER_BOUND('',#1366,.T.);
#943=FACE_OUTER_BOUND('',#1368,.T.);
#944=FACE_OUTER_BOUND('',#1369,.T.);
#945=FACE_OUTER_BOUND('',#1370,.T.);
#946=FACE_OUTER_BOUND('',#1371,.T.);
#947=FACE_OUTER_BOUND('',#1372,.T.);
#948=FACE_OUTER_BOUND('',#1373,.T.);
#949=FACE_OUTER_BOUND('',#1375,.T.);
#950=FACE_OUTER_BOUND('',#1376,.T.);
#951=FACE_OUTER_BOUND('',#1377,.T.);
#952=FACE_OUTER_BOUND('',#1383,.T.);
#953=FACE_OUTER_BOUND('',#1389,.T.);
#954=FACE_OUTER_BOUND('',#1390,.T.);
#955=FACE_OUTER_BOUND('',#1391,.T.);
#956=FACE_OUTER_BOUND('',#1392,.T.);
#957=FACE_OUTER_BOUND('',#1393,.T.);
#958=FACE_OUTER_BOUND('',#1394,.T.);
#959=FACE_OUTER_BOUND('',#1396,.T.);
#960=FACE_OUTER_BOUND('',#1397,.T.);
#961=FACE_OUTER_BOUND('',#1398,.T.);
#962=FACE_OUTER_BOUND('',#1404,.T.);
#963=FACE_OUTER_BOUND('',#1410,.T.);
#964=FACE_OUTER_BOUND('',#1411,.T.);
#965=FACE_OUTER_BOUND('',#1412,.T.);
#966=FACE_OUTER_BOUND('',#1413,.T.);
#967=FACE_OUTER_BOUND('',#1414,.T.);
#968=FACE_OUTER_BOUND('',#1415,.T.);
#969=FACE_OUTER_BOUND('',#1416,.T.);
#970=FACE_OUTER_BOUND('',#1417,.T.);
#971=FACE_OUTER_BOUND('',#1418,.T.);
#972=FACE_OUTER_BOUND('',#1419,.T.);
#973=FACE_OUTER_BOUND('',#1420,.T.);
#974=FACE_OUTER_BOUND('',#1421,.T.);
#975=FACE_OUTER_BOUND('',#1422,.T.);
#976=FACE_OUTER_BOUND('',#1423,.T.);
#977=FACE_OUTER_BOUND('',#1424,.T.);
#978=FACE_OUTER_BOUND('',#1425,.T.);
#979=FACE_OUTER_BOUND('',#1426,.T.);
#980=FACE_OUTER_BOUND('',#1428,.T.);
#981=FACE_OUTER_BOUND('',#1429,.T.);
#982=FACE_OUTER_BOUND('',#1431,.T.);
#983=FACE_OUTER_BOUND('',#1432,.T.);
#984=FACE_OUTER_BOUND('',#1433,.T.);
#985=FACE_OUTER_BOUND('',#1434,.T.);
#986=FACE_OUTER_BOUND('',#1436,.T.);
#987=FACE_OUTER_BOUND('',#1437,.T.);
#988=FACE_OUTER_BOUND('',#1438,.T.);
#989=FACE_OUTER_BOUND('',#1439,.T.);
#990=FACE_OUTER_BOUND('',#1441,.T.);
#991=FACE_OUTER_BOUND('',#1442,.T.);
#992=FACE_OUTER_BOUND('',#1443,.T.);
#993=FACE_OUTER_BOUND('',#1444,.T.);
#994=FACE_OUTER_BOUND('',#1445,.T.);
#995=FACE_OUTER_BOUND('',#1446,.T.);
#996=FACE_OUTER_BOUND('',#1447,.T.);
#997=FACE_OUTER_BOUND('',#1448,.T.);
#998=FACE_OUTER_BOUND('',#1449,.T.);
#999=FACE_OUTER_BOUND('',#1450,.T.);
#1000=FACE_OUTER_BOUND('',#1451,.T.);
#1001=FACE_OUTER_BOUND('',#1452,.T.);
#1002=FACE_OUTER_BOUND('',#1453,.T.);
#1003=FACE_OUTER_BOUND('',#1454,.T.);
#1004=FACE_OUTER_BOUND('',#1455,.T.);
#1005=FACE_OUTER_BOUND('',#1456,.T.);
#1006=FACE_OUTER_BOUND('',#1457,.T.);
#1007=FACE_OUTER_BOUND('',#1458,.T.);
#1008=FACE_OUTER_BOUND('',#1459,.T.);
#1009=FACE_OUTER_BOUND('',#1460,.T.);
#1010=FACE_OUTER_BOUND('',#1461,.T.);
#1011=FACE_OUTER_BOUND('',#1462,.T.);
#1012=FACE_OUTER_BOUND('',#1463,.T.);
#1013=FACE_OUTER_BOUND('',#1464,.T.);
#1014=FACE_OUTER_BOUND('',#1465,.T.);
#1015=FACE_OUTER_BOUND('',#1466,.T.);
#1016=FACE_OUTER_BOUND('',#1467,.T.);
#1017=FACE_OUTER_BOUND('',#1468,.T.);
#1018=FACE_OUTER_BOUND('',#1469,.T.);
#1019=FACE_OUTER_BOUND('',#1470,.T.);
#1020=FACE_OUTER_BOUND('',#1472,.T.);
#1021=FACE_OUTER_BOUND('',#1473,.T.);
#1022=FACE_OUTER_BOUND('',#1475,.T.);
#1023=FACE_OUTER_BOUND('',#1476,.T.);
#1024=FACE_OUTER_BOUND('',#1478,.T.);
#1025=FACE_OUTER_BOUND('',#1479,.T.);
#1026=FACE_OUTER_BOUND('',#1481,.T.);
#1027=FACE_OUTER_BOUND('',#1482,.T.);
#1028=FACE_OUTER_BOUND('',#1484,.T.);
#1029=FACE_OUTER_BOUND('',#1485,.T.);
#1030=FACE_OUTER_BOUND('',#1486,.T.);
#1031=FACE_OUTER_BOUND('',#1487,.T.);
#1032=FACE_OUTER_BOUND('',#1488,.T.);
#1033=FACE_OUTER_BOUND('',#1489,.T.);
#1034=FACE_OUTER_BOUND('',#1491,.T.);
#1035=FACE_OUTER_BOUND('',#1492,.T.);
#1036=FACE_OUTER_BOUND('',#1493,.T.);
#1037=FACE_OUTER_BOUND('',#1494,.T.);
#1038=FACE_OUTER_BOUND('',#1495,.T.);
#1039=FACE_OUTER_BOUND('',#1496,.T.);
#1040=FACE_OUTER_BOUND('',#1497,.T.);
#1041=FACE_OUTER_BOUND('',#1498,.T.);
#1042=FACE_OUTER_BOUND('',#1499,.T.);
#1043=FACE_OUTER_BOUND('',#1500,.T.);
#1044=FACE_OUTER_BOUND('',#1501,.T.);
#1045=FACE_OUTER_BOUND('',#1502,.T.);
#1046=FACE_OUTER_BOUND('',#1503,.T.);
#1047=FACE_OUTER_BOUND('',#1504,.T.);
#1048=FACE_OUTER_BOUND('',#1505,.T.);
#1049=FACE_OUTER_BOUND('',#1506,.T.);
#1050=FACE_OUTER_BOUND('',#1507,.T.);
#1051=FACE_OUTER_BOUND('',#1509,.T.);
#1052=FACE_OUTER_BOUND('',#1510,.T.);
#1053=FACE_OUTER_BOUND('',#1511,.T.);
#1054=FACE_OUTER_BOUND('',#1512,.T.);
#1055=FACE_OUTER_BOUND('',#1513,.T.);
#1056=FACE_OUTER_BOUND('',#1514,.T.);
#1057=FACE_OUTER_BOUND('',#1515,.T.);
#1058=FACE_OUTER_BOUND('',#1516,.T.);
#1059=FACE_OUTER_BOUND('',#1517,.T.);
#1060=FACE_OUTER_BOUND('',#1518,.T.);
#1061=FACE_OUTER_BOUND('',#1519,.T.);
#1062=FACE_OUTER_BOUND('',#1520,.T.);
#1063=FACE_OUTER_BOUND('',#1521,.T.);
#1064=FACE_OUTER_BOUND('',#1522,.T.);
#1065=FACE_OUTER_BOUND('',#1523,.T.);
#1066=FACE_OUTER_BOUND('',#1524,.T.);
#1067=FACE_OUTER_BOUND('',#1525,.T.);
#1068=FACE_OUTER_BOUND('',#1526,.T.);
#1069=FACE_OUTER_BOUND('',#1527,.T.);
#1070=FACE_OUTER_BOUND('',#1528,.T.);
#1071=FACE_OUTER_BOUND('',#1529,.T.);
#1072=FACE_OUTER_BOUND('',#1530,.T.);
#1073=FACE_OUTER_BOUND('',#1531,.T.);
#1074=FACE_OUTER_BOUND('',#1533,.T.);
#1075=FACE_OUTER_BOUND('',#1535,.T.);
#1076=FACE_OUTER_BOUND('',#1536,.T.);
#1077=FACE_OUTER_BOUND('',#1538,.T.);
#1078=FACE_OUTER_BOUND('',#1540,.T.);
#1079=FACE_OUTER_BOUND('',#1541,.T.);
#1080=FACE_OUTER_BOUND('',#1542,.T.);
#1081=FACE_OUTER_BOUND('',#1543,.T.);
#1082=FACE_OUTER_BOUND('',#1544,.T.);
#1083=FACE_OUTER_BOUND('',#1546,.T.);
#1084=FACE_OUTER_BOUND('',#1548,.T.);
#1085=FACE_OUTER_BOUND('',#1549,.T.);
#1086=FACE_OUTER_BOUND('',#1550,.T.);
#1087=FACE_OUTER_BOUND('',#1551,.T.);
#1088=FACE_OUTER_BOUND('',#1553,.T.);
#1089=FACE_OUTER_BOUND('',#1555,.T.);
#1090=FACE_OUTER_BOUND('',#1557,.T.);
#1091=FACE_OUTER_BOUND('',#1559,.T.);
#1092=FACE_OUTER_BOUND('',#1560,.T.);
#1093=FACE_OUTER_BOUND('',#1561,.T.);
#1094=FACE_OUTER_BOUND('',#1562,.T.);
#1095=FACE_OUTER_BOUND('',#1563,.T.);
#1096=FACE_OUTER_BOUND('',#1564,.T.);
#1097=FACE_OUTER_BOUND('',#1565,.T.);
#1098=FACE_OUTER_BOUND('',#1566,.T.);
#1099=FACE_OUTER_BOUND('',#1567,.T.);
#1100=FACE_OUTER_BOUND('',#1569,.T.);
#1101=FACE_OUTER_BOUND('',#1570,.T.);
#1102=FACE_OUTER_BOUND('',#1571,.T.);
#1103=FACE_OUTER_BOUND('',#1572,.T.);
#1104=FACE_OUTER_BOUND('',#1573,.T.);
#1105=FACE_OUTER_BOUND('',#1574,.T.);
#1106=FACE_OUTER_BOUND('',#1575,.T.);
#1107=FACE_OUTER_BOUND('',#1577,.T.);
#1108=FACE_OUTER_BOUND('',#1579,.T.);
#1109=FACE_OUTER_BOUND('',#1581,.T.);
#1110=FACE_OUTER_BOUND('',#1582,.T.);
#1111=FACE_OUTER_BOUND('',#1583,.T.);
#1112=FACE_OUTER_BOUND('',#1584,.T.);
#1113=FACE_OUTER_BOUND('',#1585,.T.);
#1114=FACE_OUTER_BOUND('',#1586,.T.);
#1115=FACE_OUTER_BOUND('',#1587,.T.);
#1116=FACE_OUTER_BOUND('',#1589,.T.);
#1117=FACE_OUTER_BOUND('',#1591,.T.);
#1118=FACE_OUTER_BOUND('',#1592,.T.);
#1119=FACE_OUTER_BOUND('',#1593,.T.);
#1120=FACE_OUTER_BOUND('',#1595,.T.);
#1121=FACE_OUTER_BOUND('',#1596,.T.);
#1122=FACE_OUTER_BOUND('',#1598,.T.);
#1123=FACE_OUTER_BOUND('',#1599,.T.);
#1124=FACE_OUTER_BOUND('',#1602,.T.);
#1125=FACE_OUTER_BOUND('',#1604,.T.);
#1126=FACE_OUTER_BOUND('',#1605,.T.);
#1127=FACE_OUTER_BOUND('',#1607,.T.);
#1128=FACE_OUTER_BOUND('',#1608,.T.);
#1129=FACE_OUTER_BOUND('',#1609,.T.);
#1130=FACE_OUTER_BOUND('',#1611,.T.);
#1131=FACE_OUTER_BOUND('',#1613,.T.);
#1132=FACE_OUTER_BOUND('',#1614,.T.);
#1133=FACE_OUTER_BOUND('',#1616,.T.);
#1134=FACE_OUTER_BOUND('',#1617,.T.);
#1135=FACE_OUTER_BOUND('',#1618,.T.);
#1136=FACE_OUTER_BOUND('',#1620,.T.);
#1137=FACE_OUTER_BOUND('',#1622,.T.);
#1138=FACE_OUTER_BOUND('',#1623,.T.);
#1139=FACE_OUTER_BOUND('',#1624,.T.);
#1140=FACE_OUTER_BOUND('',#1625,.T.);
#1141=FACE_OUTER_BOUND('',#1626,.T.);
#1142=FACE_OUTER_BOUND('',#1627,.T.);
#1143=FACE_OUTER_BOUND('',#1628,.T.);
#1144=FACE_OUTER_BOUND('',#1629,.T.);
#1145=FACE_OUTER_BOUND('',#1630,.T.);
#1146=FACE_OUTER_BOUND('',#1631,.T.);
#1147=FACE_OUTER_BOUND('',#1632,.T.);
#1148=FACE_OUTER_BOUND('',#1633,.T.);
#1149=FACE_OUTER_BOUND('',#1634,.T.);
#1150=FACE_OUTER_BOUND('',#1635,.T.);
#1151=FACE_OUTER_BOUND('',#1636,.T.);
#1152=FACE_OUTER_BOUND('',#1637,.T.);
#1153=FACE_OUTER_BOUND('',#1638,.T.);
#1154=FACE_OUTER_BOUND('',#1639,.T.);
#1155=FACE_OUTER_BOUND('',#1641,.T.);
#1156=FACE_OUTER_BOUND('',#1642,.T.);
#1157=FACE_OUTER_BOUND('',#1643,.T.);
#1158=FACE_OUTER_BOUND('',#1644,.T.);
#1159=FACE_OUTER_BOUND('',#1645,.T.);
#1160=FACE_OUTER_BOUND('',#1646,.T.);
#1161=FACE_OUTER_BOUND('',#1647,.T.);
#1162=FACE_OUTER_BOUND('',#1648,.T.);
#1163=FACE_OUTER_BOUND('',#1649,.T.);
#1164=FACE_OUTER_BOUND('',#1651,.T.);
#1165=FACE_OUTER_BOUND('',#1652,.T.);
#1166=FACE_OUTER_BOUND('',#1654,.T.);
#1167=FACE_OUTER_BOUND('',#1655,.T.);
#1168=FACE_OUTER_BOUND('',#1656,.T.);
#1169=FACE_OUTER_BOUND('',#1657,.T.);
#1170=FACE_OUTER_BOUND('',#1659,.T.);
#1171=FACE_OUTER_BOUND('',#1660,.T.);
#1172=FACE_OUTER_BOUND('',#1661,.T.);
#1173=FACE_OUTER_BOUND('',#1662,.T.);
#1174=FACE_OUTER_BOUND('',#1664,.T.);
#1175=FACE_OUTER_BOUND('',#1665,.T.);
#1176=FACE_OUTER_BOUND('',#1666,.T.);
#1177=FACE_OUTER_BOUND('',#1667,.T.);
#1178=FACE_OUTER_BOUND('',#1668,.T.);
#1179=FACE_OUTER_BOUND('',#1669,.T.);
#1180=FACE_OUTER_BOUND('',#1670,.T.);
#1181=FACE_OUTER_BOUND('',#1671,.T.);
#1182=FACE_OUTER_BOUND('',#1672,.T.);
#1183=FACE_OUTER_BOUND('',#1673,.T.);
#1184=FACE_OUTER_BOUND('',#1674,.T.);
#1185=FACE_OUTER_BOUND('',#1675,.T.);
#1186=FACE_OUTER_BOUND('',#1676,.T.);
#1187=FACE_OUTER_BOUND('',#1677,.T.);
#1188=FACE_OUTER_BOUND('',#1678,.T.);
#1189=FACE_OUTER_BOUND('',#1679,.T.);
#1190=FACE_OUTER_BOUND('',#1680,.T.);
#1191=FACE_OUTER_BOUND('',#1681,.T.);
#1192=FACE_OUTER_BOUND('',#1682,.T.);
#1193=FACE_OUTER_BOUND('',#1683,.T.);
#1194=FACE_OUTER_BOUND('',#1684,.T.);
#1195=FACE_OUTER_BOUND('',#1685,.T.);
#1196=FACE_OUTER_BOUND('',#1686,.T.);
#1197=FACE_OUTER_BOUND('',#1687,.T.);
#1198=FACE_OUTER_BOUND('',#1688,.T.);
#1199=FACE_OUTER_BOUND('',#1689,.T.);
#1200=FACE_OUTER_BOUND('',#1690,.T.);
#1201=FACE_OUTER_BOUND('',#1692,.T.);
#1202=FACE_OUTER_BOUND('',#1693,.T.);
#1203=FACE_OUTER_BOUND('',#1695,.T.);
#1204=FACE_OUTER_BOUND('',#1696,.T.);
#1205=FACE_OUTER_BOUND('',#1698,.T.);
#1206=FACE_OUTER_BOUND('',#1699,.T.);
#1207=FACE_OUTER_BOUND('',#1701,.T.);
#1208=FACE_OUTER_BOUND('',#1702,.T.);
#1209=FACE_OUTER_BOUND('',#1704,.T.);
#1210=FACE_OUTER_BOUND('',#1705,.T.);
#1211=FACE_OUTER_BOUND('',#1706,.T.);
#1212=FACE_OUTER_BOUND('',#1707,.T.);
#1213=FACE_OUTER_BOUND('',#1708,.T.);
#1214=FACE_OUTER_BOUND('',#1710,.T.);
#1215=FACE_OUTER_BOUND('',#1711,.T.);
#1216=FACE_OUTER_BOUND('',#1713,.T.);
#1217=FACE_OUTER_BOUND('',#1715,.T.);
#1218=FACE_OUTER_BOUND('',#1717,.T.);
#1219=FACE_OUTER_BOUND('',#1718,.T.);
#1220=FACE_OUTER_BOUND('',#1720,.T.);
#1221=FACE_OUTER_BOUND('',#1721,.T.);
#1222=FACE_OUTER_BOUND('',#1722,.T.);
#1223=FACE_OUTER_BOUND('',#1724,.T.);
#1224=FACE_OUTER_BOUND('',#1725,.T.);
#1225=FACE_OUTER_BOUND('',#1726,.T.);
#1226=FACE_OUTER_BOUND('',#1727,.T.);
#1227=FACE_OUTER_BOUND('',#1728,.T.);
#1228=FACE_OUTER_BOUND('',#1729,.T.);
#1229=FACE_OUTER_BOUND('',#1731,.T.);
#1230=FACE_OUTER_BOUND('',#1733,.T.);
#1231=FACE_OUTER_BOUND('',#1734,.T.);
#1232=FACE_OUTER_BOUND('',#1735,.T.);
#1233=FACE_OUTER_BOUND('',#1737,.T.);
#1234=FACE_OUTER_BOUND('',#1739,.T.);
#1235=FACE_OUTER_BOUND('',#1740,.T.);
#1236=FACE_OUTER_BOUND('',#1741,.T.);
#1237=FACE_OUTER_BOUND('',#1743,.T.);
#1238=FACE_OUTER_BOUND('',#1745,.T.);
#1239=FACE_OUTER_BOUND('',#1746,.T.);
#1240=FACE_OUTER_BOUND('',#1747,.T.);
#1241=FACE_OUTER_BOUND('',#1749,.T.);
#1242=FACE_OUTER_BOUND('',#1751,.T.);
#1243=FACE_OUTER_BOUND('',#1752,.T.);
#1244=FACE_OUTER_BOUND('',#1753,.T.);
#1245=FACE_OUTER_BOUND('',#1755,.T.);
#1246=FACE_OUTER_BOUND('',#1757,.T.);
#1247=FACE_OUTER_BOUND('',#1758,.T.);
#1248=FACE_OUTER_BOUND('',#1759,.T.);
#1249=FACE_OUTER_BOUND('',#1761,.T.);
#1250=FACE_OUTER_BOUND('',#1763,.T.);
#1251=FACE_OUTER_BOUND('',#1764,.T.);
#1252=FACE_OUTER_BOUND('',#1765,.T.);
#1253=FACE_OUTER_BOUND('',#1767,.T.);
#1254=FACE_OUTER_BOUND('',#1769,.T.);
#1255=FACE_OUTER_BOUND('',#1770,.T.);
#1256=FACE_OUTER_BOUND('',#1771,.T.);
#1257=FACE_OUTER_BOUND('',#1772,.T.);
#1258=FACE_OUTER_BOUND('',#1773,.T.);
#1259=FACE_OUTER_BOUND('',#1774,.T.);
#1260=FACE_OUTER_BOUND('',#1775,.T.);
#1261=FACE_OUTER_BOUND('',#1776,.T.);
#1262=FACE_OUTER_BOUND('',#1777,.T.);
#1263=FACE_OUTER_BOUND('',#1778,.T.);
#1264=FACE_OUTER_BOUND('',#1779,.T.);
#1265=FACE_OUTER_BOUND('',#1780,.T.);
#1266=FACE_OUTER_BOUND('',#1781,.T.);
#1267=FACE_OUTER_BOUND('',#1782,.T.);
#1268=FACE_OUTER_BOUND('',#1784,.T.);
#1269=FACE_OUTER_BOUND('',#1785,.T.);
#1270=EDGE_LOOP('',(#4351,#4352,#4353,#4354));
#1271=EDGE_LOOP('',(#4355,#4356,#4357,#4358));
#1272=EDGE_LOOP('',(#4359,#4360,#4361,#4362));
#1273=EDGE_LOOP('',(#4363,#4364,#4365,#4366));
#1274=EDGE_LOOP('',(#4367,#4368,#4369,#4370));
#1275=EDGE_LOOP('',(#4371,#4372,#4373,#4374));
#1276=EDGE_LOOP('',(#4375,#4376,#4377,#4378));
#1277=EDGE_LOOP('',(#4379,#4380,#4381,#4382));
#1278=EDGE_LOOP('',(#4383,#4384,#4385,#4386));
#1279=EDGE_LOOP('',(#4387));
#1280=EDGE_LOOP('',(#4388));
#1281=EDGE_LOOP('',(#4389));
#1282=EDGE_LOOP('',(#4390));
#1283=EDGE_LOOP('',(#4391,#4392,#4393,#4394));
#1284=EDGE_LOOP('',(#4395));
#1285=EDGE_LOOP('',(#4396));
#1286=EDGE_LOOP('',(#4397));
#1287=EDGE_LOOP('',(#4398));
#1288=EDGE_LOOP('',(#4399,#4400,#4401,#4402));
#1289=EDGE_LOOP('',(#4403));
#1290=EDGE_LOOP('',(#4404,#4405,#4406,#4407));
#1291=EDGE_LOOP('',(#4408));
#1292=EDGE_LOOP('',(#4409,#4410,#4411,#4412));
#1293=EDGE_LOOP('',(#4413));
#1294=EDGE_LOOP('',(#4414,#4415,#4416,#4417));
#1295=EDGE_LOOP('',(#4418));
#1296=EDGE_LOOP('',(#4419,#4420,#4421,#4422));
#1297=EDGE_LOOP('',(#4423));
#1298=EDGE_LOOP('',(#4424,#4425,#4426,#4427));
#1299=EDGE_LOOP('',(#4428));
#1300=EDGE_LOOP('',(#4429,#4430,#4431,#4432));
#1301=EDGE_LOOP('',(#4433));
#1302=EDGE_LOOP('',(#4434,#4435,#4436,#4437));
#1303=EDGE_LOOP('',(#4438));
#1304=EDGE_LOOP('',(#4439,#4440,#4441,#4442));
#1305=EDGE_LOOP('',(#4443,#4444,#4445,#4446));
#1306=EDGE_LOOP('',(#4447,#4448,#4449,#4450));
#1307=EDGE_LOOP('',(#4451));
#1308=EDGE_LOOP('',(#4452,#4453,#4454,#4455));
#1309=EDGE_LOOP('',(#4456,#4457,#4458,#4459));
#1310=EDGE_LOOP('',(#4460,#4461,#4462,#4463));
#1311=EDGE_LOOP('',(#4464));
#1312=EDGE_LOOP('',(#4465,#4466,#4467,#4468));
#1313=EDGE_LOOP('',(#4469,#4470,#4471,#4472));
#1314=EDGE_LOOP('',(#4473,#4474,#4475,#4476));
#1315=EDGE_LOOP('',(#4477));
#1316=EDGE_LOOP('',(#4478,#4479,#4480,#4481));
#1317=EDGE_LOOP('',(#4482,#4483,#4484,#4485));
#1318=EDGE_LOOP('',(#4486,#4487,#4488,#4489));
#1319=EDGE_LOOP('',(#4490));
#1320=EDGE_LOOP('',(#4491,#4492,#4493,#4494));
#1321=EDGE_LOOP('',(#4495,#4496,#4497,#4498));
#1322=EDGE_LOOP('',(#4499,#4500,#4501,#4502));
#1323=EDGE_LOOP('',(#4503,#4504,#4505,#4506));
#1324=EDGE_LOOP('',(#4507,#4508,#4509,#4510,#4511,#4512,#4513,#4514,#4515,
#4516,#4517,#4518,#4519,#4520));
#1325=EDGE_LOOP('',(#4521,#4522,#4523,#4524));
#1326=EDGE_LOOP('',(#4525,#4526,#4527,#4528));
#1327=EDGE_LOOP('',(#4529,#4530,#4531,#4532,#4533,#4534,#4535,#4536,#4537,
#4538,#4539,#4540,#4541,#4542));
#1328=EDGE_LOOP('',(#4543,#4544,#4545,#4546));
#1329=EDGE_LOOP('',(#4547,#4548,#4549,#4550));
#1330=EDGE_LOOP('',(#4551,#4552,#4553,#4554));
#1331=EDGE_LOOP('',(#4555,#4556,#4557,#4558));
#1332=EDGE_LOOP('',(#4559,#4560,#4561,#4562));
#1333=EDGE_LOOP('',(#4563,#4564,#4565,#4566));
#1334=EDGE_LOOP('',(#4567,#4568,#4569,#4570));
#1335=EDGE_LOOP('',(#4571,#4572,#4573,#4574));
#1336=EDGE_LOOP('',(#4575));
#1337=EDGE_LOOP('',(#4576));
#1338=EDGE_LOOP('',(#4577,#4578,#4579,#4580));
#1339=EDGE_LOOP('',(#4581,#4582,#4583,#4584,#4585,#4586,#4587,#4588,#4589,
#4590,#4591,#4592,#4593,#4594));
#1340=EDGE_LOOP('',(#4595,#4596,#4597,#4598));
#1341=EDGE_LOOP('',(#4599,#4600,#4601,#4602));
#1342=EDGE_LOOP('',(#4603));
#1343=EDGE_LOOP('',(#4604));
#1344=EDGE_LOOP('',(#4605,#4606,#4607,#4608));
#1345=EDGE_LOOP('',(#4609,#4610,#4611,#4612,#4613,#4614,#4615,#4616,#4617,
#4618,#4619,#4620,#4621,#4622));
#1346=EDGE_LOOP('',(#4623,#4624,#4625,#4626));
#1347=EDGE_LOOP('',(#4627,#4628,#4629,#4630));
#1348=EDGE_LOOP('',(#4631,#4632,#4633,#4634));
#1349=EDGE_LOOP('',(#4635,#4636,#4637,#4638));
#1350=EDGE_LOOP('',(#4639));
#1351=EDGE_LOOP('',(#4640));
#1352=EDGE_LOOP('',(#4641));
#1353=EDGE_LOOP('',(#4642));
#1354=EDGE_LOOP('',(#4643));
#1355=EDGE_LOOP('',(#4644));
#1356=EDGE_LOOP('',(#4645));
#1357=EDGE_LOOP('',(#4646));
#1358=EDGE_LOOP('',(#4647));
#1359=EDGE_LOOP('',(#4648));
#1360=EDGE_LOOP('',(#4649));
#1361=EDGE_LOOP('',(#4650));
#1362=EDGE_LOOP('',(#4651,#4652,#4653,#4654));
#1363=EDGE_LOOP('',(#4655,#4656,#4657,#4658));
#1364=EDGE_LOOP('',(#4659));
#1365=EDGE_LOOP('',(#4660));
#1366=EDGE_LOOP('',(#4661));
#1367=EDGE_LOOP('',(#4662));
#1368=EDGE_LOOP('',(#4663,#4664,#4665,#4666));
#1369=EDGE_LOOP('',(#4667,#4668,#4669,#4670));
#1370=EDGE_LOOP('',(#4671,#4672,#4673,#4674));
#1371=EDGE_LOOP('',(#4675,#4676,#4677,#4678));
#1372=EDGE_LOOP('',(#4679,#4680,#4681,#4682));
#1373=EDGE_LOOP('',(#4683));
#1374=EDGE_LOOP('',(#4684));
#1375=EDGE_LOOP('',(#4685,#4686,#4687,#4688));
#1376=EDGE_LOOP('',(#4689,#4690,#4691,#4692));
#1377=EDGE_LOOP('',(#4693));
#1378=EDGE_LOOP('',(#4694));
#1379=EDGE_LOOP('',(#4695));
#1380=EDGE_LOOP('',(#4696));
#1381=EDGE_LOOP('',(#4697));
#1382=EDGE_LOOP('',(#4698));
#1383=EDGE_LOOP('',(#4699));
#1384=EDGE_LOOP('',(#4700));
#1385=EDGE_LOOP('',(#4701));
#1386=EDGE_LOOP('',(#4702));
#1387=EDGE_LOOP('',(#4703));
#1388=EDGE_LOOP('',(#4704));
#1389=EDGE_LOOP('',(#4705,#4706,#4707,#4708));
#1390=EDGE_LOOP('',(#4709,#4710,#4711,#4712));
#1391=EDGE_LOOP('',(#4713,#4714,#4715,#4716));
#1392=EDGE_LOOP('',(#4717,#4718,#4719,#4720));
#1393=EDGE_LOOP('',(#4721,#4722,#4723,#4724));
#1394=EDGE_LOOP('',(#4725));
#1395=EDGE_LOOP('',(#4726));
#1396=EDGE_LOOP('',(#4727,#4728,#4729,#4730));
#1397=EDGE_LOOP('',(#4731,#4732,#4733,#4734));
#1398=EDGE_LOOP('',(#4735));
#1399=EDGE_LOOP('',(#4736));
#1400=EDGE_LOOP('',(#4737));
#1401=EDGE_LOOP('',(#4738));
#1402=EDGE_LOOP('',(#4739));
#1403=EDGE_LOOP('',(#4740));
#1404=EDGE_LOOP('',(#4741));
#1405=EDGE_LOOP('',(#4742));
#1406=EDGE_LOOP('',(#4743));
#1407=EDGE_LOOP('',(#4744));
#1408=EDGE_LOOP('',(#4745));
#1409=EDGE_LOOP('',(#4746));
#1410=EDGE_LOOP('',(#4747,#4748,#4749,#4750));
#1411=EDGE_LOOP('',(#4751,#4752,#4753,#4754));
#1412=EDGE_LOOP('',(#4755,#4756,#4757,#4758));
#1413=EDGE_LOOP('',(#4759,#4760,#4761,#4762));
#1414=EDGE_LOOP('',(#4763,#4764,#4765,#4766));
#1415=EDGE_LOOP('',(#4767,#4768,#4769,#4770));
#1416=EDGE_LOOP('',(#4771,#4772,#4773,#4774));
#1417=EDGE_LOOP('',(#4775,#4776,#4777,#4778));
#1418=EDGE_LOOP('',(#4779,#4780,#4781,#4782));
#1419=EDGE_LOOP('',(#4783,#4784,#4785,#4786));
#1420=EDGE_LOOP('',(#4787,#4788,#4789,#4790));
#1421=EDGE_LOOP('',(#4791,#4792,#4793,#4794));
#1422=EDGE_LOOP('',(#4795,#4796,#4797,#4798,#4799,#4800));
#1423=EDGE_LOOP('',(#4801,#4802,#4803,#4804,#4805));
#1424=EDGE_LOOP('',(#4806,#4807,#4808,#4809));
#1425=EDGE_LOOP('',(#4810,#4811,#4812,#4813));
#1426=EDGE_LOOP('',(#4814));
#1427=EDGE_LOOP('',(#4815));
#1428=EDGE_LOOP('',(#4816,#4817,#4818,#4819,#4820));
#1429=EDGE_LOOP('',(#4821));
#1430=EDGE_LOOP('',(#4822));
#1431=EDGE_LOOP('',(#4823,#4824,#4825,#4826));
#1432=EDGE_LOOP('',(#4827,#4828,#4829,#4830,#4831,#4832));
#1433=EDGE_LOOP('',(#4833,#4834,#4835,#4836,#4837));
#1434=EDGE_LOOP('',(#4838));
#1435=EDGE_LOOP('',(#4839));
#1436=EDGE_LOOP('',(#4840,#4841,#4842,#4843));
#1437=EDGE_LOOP('',(#4844,#4845,#4846,#4847));
#1438=EDGE_LOOP('',(#4848,#4849,#4850,#4851));
#1439=EDGE_LOOP('',(#4852));
#1440=EDGE_LOOP('',(#4853));
#1441=EDGE_LOOP('',(#4854,#4855,#4856,#4857,#4858));
#1442=EDGE_LOOP('',(#4859,#4860));
#1443=EDGE_LOOP('',(#4861,#4862));
#1444=EDGE_LOOP('',(#4863,#4864));
#1445=EDGE_LOOP('',(#4865,#4866));
#1446=EDGE_LOOP('',(#4867,#4868));
#1447=EDGE_LOOP('',(#4869,#4870));
#1448=EDGE_LOOP('',(#4871,#4872));
#1449=EDGE_LOOP('',(#4873,#4874));
#1450=EDGE_LOOP('',(#4875,#4876));
#1451=EDGE_LOOP('',(#4877,#4878,#4879,#4880));
#1452=EDGE_LOOP('',(#4881,#4882,#4883,#4884,#4885,#4886,#4887,#4888,#4889,
#4890,#4891,#4892,#4893,#4894,#4895,#4896,#4897,#4898,#4899,#4900,#4901,
#4902));
#1453=EDGE_LOOP('',(#4903,#4904,#4905,#4906));
#1454=EDGE_LOOP('',(#4907,#4908,#4909,#4910));
#1455=EDGE_LOOP('',(#4911,#4912,#4913,#4914));
#1456=EDGE_LOOP('',(#4915,#4916,#4917,#4918));
#1457=EDGE_LOOP('',(#4919,#4920,#4921,#4922));
#1458=EDGE_LOOP('',(#4923,#4924,#4925,#4926));
#1459=EDGE_LOOP('',(#4927,#4928,#4929,#4930,#4931,#4932));
#1460=EDGE_LOOP('',(#4933,#4934,#4935,#4936));
#1461=EDGE_LOOP('',(#4937,#4938,#4939,#4940));
#1462=EDGE_LOOP('',(#4941,#4942,#4943,#4944));
#1463=EDGE_LOOP('',(#4945,#4946,#4947,#4948));
#1464=EDGE_LOOP('',(#4949,#4950,#4951,#4952));
#1465=EDGE_LOOP('',(#4953,#4954,#4955,#4956));
#1466=EDGE_LOOP('',(#4957,#4958,#4959,#4960));
#1467=EDGE_LOOP('',(#4961,#4962,#4963,#4964,#4965,#4966,#4967,#4968,#4969,
#4970,#4971,#4972,#4973,#4974,#4975,#4976,#4977,#4978,#4979,#4980,#4981,
#4982));
#1468=EDGE_LOOP('',(#4983,#4984,#4985,#4986));
#1469=EDGE_LOOP('',(#4987,#4988,#4989,#4990));
#1470=EDGE_LOOP('',(#4991));
#1471=EDGE_LOOP('',(#4992));
#1472=EDGE_LOOP('',(#4993,#4994,#4995,#4996));
#1473=EDGE_LOOP('',(#4997));
#1474=EDGE_LOOP('',(#4998));
#1475=EDGE_LOOP('',(#4999,#5000,#5001,#5002));
#1476=EDGE_LOOP('',(#5003));
#1477=EDGE_LOOP('',(#5004));
#1478=EDGE_LOOP('',(#5005,#5006,#5007,#5008));
#1479=EDGE_LOOP('',(#5009));
#1480=EDGE_LOOP('',(#5010));
#1481=EDGE_LOOP('',(#5011,#5012,#5013,#5014));
#1482=EDGE_LOOP('',(#5015));
#1483=EDGE_LOOP('',(#5016));
#1484=EDGE_LOOP('',(#5017,#5018,#5019,#5020));
#1485=EDGE_LOOP('',(#5021));
#1486=EDGE_LOOP('',(#5022,#5023,#5024,#5025));
#1487=EDGE_LOOP('',(#5026,#5027,#5028,#5029));
#1488=EDGE_LOOP('',(#5030,#5031,#5032,#5033));
#1489=EDGE_LOOP('',(#5034));
#1490=EDGE_LOOP('',(#5035));
#1491=EDGE_LOOP('',(#5036,#5037,#5038,#5039));
#1492=EDGE_LOOP('',(#5040,#5041,#5042,#5043));
#1493=EDGE_LOOP('',(#5044,#5045,#5046,#5047));
#1494=EDGE_LOOP('',(#5048));
#1495=EDGE_LOOP('',(#5049,#5050,#5051,#5052));
#1496=EDGE_LOOP('',(#5053,#5054,#5055,#5056));
#1497=EDGE_LOOP('',(#5057,#5058,#5059,#5060));
#1498=EDGE_LOOP('',(#5061,#5062,#5063,#5064));
#1499=EDGE_LOOP('',(#5065,#5066,#5067,#5068));
#1500=EDGE_LOOP('',(#5069,#5070,#5071,#5072));
#1501=EDGE_LOOP('',(#5073,#5074,#5075,#5076,#5077,#5078));
#1502=EDGE_LOOP('',(#5079,#5080,#5081,#5082,#5083,#5084));
#1503=EDGE_LOOP('',(#5085));
#1504=EDGE_LOOP('',(#5086,#5087,#5088,#5089));
#1505=EDGE_LOOP('',(#5090,#5091,#5092,#5093));
#1506=EDGE_LOOP('',(#5094,#5095,#5096,#5097));
#1507=EDGE_LOOP('',(#5098));
#1508=EDGE_LOOP('',(#5099));
#1509=EDGE_LOOP('',(#5100,#5101,#5102,#5103));
#1510=EDGE_LOOP('',(#5104,#5105,#5106,#5107));
#1511=EDGE_LOOP('',(#5108,#5109,#5110,#5111));
#1512=EDGE_LOOP('',(#5112));
#1513=EDGE_LOOP('',(#5113,#5114,#5115,#5116));
#1514=EDGE_LOOP('',(#5117,#5118,#5119,#5120));
#1515=EDGE_LOOP('',(#5121,#5122,#5123,#5124));
#1516=EDGE_LOOP('',(#5125,#5126,#5127,#5128));
#1517=EDGE_LOOP('',(#5129,#5130,#5131,#5132));
#1518=EDGE_LOOP('',(#5133,#5134,#5135,#5136));
#1519=EDGE_LOOP('',(#5137,#5138,#5139,#5140,#5141,#5142));
#1520=EDGE_LOOP('',(#5143,#5144,#5145,#5146,#5147,#5148));
#1521=EDGE_LOOP('',(#5149,#5150,#5151,#5152));
#1522=EDGE_LOOP('',(#5153,#5154,#5155,#5156));
#1523=EDGE_LOOP('',(#5157,#5158,#5159,#5160));
#1524=EDGE_LOOP('',(#5161,#5162,#5163,#5164));
#1525=EDGE_LOOP('',(#5165,#5166,#5167,#5168));
#1526=EDGE_LOOP('',(#5169,#5170,#5171,#5172));
#1527=EDGE_LOOP('',(#5173,#5174,#5175,#5176));
#1528=EDGE_LOOP('',(#5177,#5178,#5179,#5180));
#1529=EDGE_LOOP('',(#5181,#5182,#5183,#5184));
#1530=EDGE_LOOP('',(#5185,#5186,#5187,#5188));
#1531=EDGE_LOOP('',(#5189));
#1532=EDGE_LOOP('',(#5190));
#1533=EDGE_LOOP('',(#5191));
#1534=EDGE_LOOP('',(#5192));
#1535=EDGE_LOOP('',(#5193,#5194,#5195,#5196));
#1536=EDGE_LOOP('',(#5197,#5198,#5199,#5200));
#1537=EDGE_LOOP('',(#5201,#5202,#5203,#5204));
#1538=EDGE_LOOP('',(#5205,#5206,#5207,#5208));
#1539=EDGE_LOOP('',(#5209,#5210,#5211,#5212));
#1540=EDGE_LOOP('',(#5213));
#1541=EDGE_LOOP('',(#5214));
#1542=EDGE_LOOP('',(#5215,#5216,#5217,#5218));
#1543=EDGE_LOOP('',(#5219,#5220,#5221,#5222));
#1544=EDGE_LOOP('',(#5223));
#1545=EDGE_LOOP('',(#5224));
#1546=EDGE_LOOP('',(#5225));
#1547=EDGE_LOOP('',(#5226));
#1548=EDGE_LOOP('',(#5227,#5228));
#1549=EDGE_LOOP('',(#5229,#5230,#5231,#5232,#5233,#5234,#5235,#5236,#5237));
#1550=EDGE_LOOP('',(#5238,#5239,#5240));
#1551=EDGE_LOOP('',(#5241,#5242,#5243,#5244));
#1552=EDGE_LOOP('',(#5245,#5246,#5247,#5248));
#1553=EDGE_LOOP('',(#5249,#5250,#5251,#5252));
#1554=EDGE_LOOP('',(#5253,#5254));
#1555=EDGE_LOOP('',(#5255));
#1556=EDGE_LOOP('',(#5256));
#1557=EDGE_LOOP('',(#5257));
#1558=EDGE_LOOP('',(#5258));
#1559=EDGE_LOOP('',(#5259,#5260));
#1560=EDGE_LOOP('',(#5261,#5262,#5263,#5264,#5265,#5266,#5267,#5268,#5269));
#1561=EDGE_LOOP('',(#5270,#5271,#5272));
#1562=EDGE_LOOP('',(#5273,#5274,#5275,#5276));
#1563=EDGE_LOOP('',(#5277,#5278,#5279,#5280,#5281,#5282));
#1564=EDGE_LOOP('',(#5283,#5284,#5285,#5286,#5287,#5288));
#1565=EDGE_LOOP('',(#5289,#5290,#5291,#5292));
#1566=EDGE_LOOP('',(#5293,#5294,#5295,#5296));
#1567=EDGE_LOOP('',(#5297));
#1568=EDGE_LOOP('',(#5298,#5299,#5300,#5301));
#1569=EDGE_LOOP('',(#5302,#5303,#5304,#5305));
#1570=EDGE_LOOP('',(#5306,#5307,#5308,#5309));
#1571=EDGE_LOOP('',(#5310,#5311,#5312,#5313));
#1572=EDGE_LOOP('',(#5314,#5315,#5316,#5317));
#1573=EDGE_LOOP('',(#5318,#5319,#5320,#5321));
#1574=EDGE_LOOP('',(#5322,#5323,#5324,#5325));
#1575=EDGE_LOOP('',(#5326));
#1576=EDGE_LOOP('',(#5327,#5328,#5329,#5330));
#1577=EDGE_LOOP('',(#5331,#5332,#5333,#5334));
#1578=EDGE_LOOP('',(#5335,#5336,#5337,#5338));
#1579=EDGE_LOOP('',(#5339,#5340,#5341,#5342));
#1580=EDGE_LOOP('',(#5343,#5344));
#1581=EDGE_LOOP('',(#5345,#5346));
#1582=EDGE_LOOP('',(#5347,#5348,#5349,#5350,#5351,#5352,#5353,#5354,#5355));
#1583=EDGE_LOOP('',(#5356,#5357,#5358));
#1584=EDGE_LOOP('',(#5359,#5360,#5361,#5362));
#1585=EDGE_LOOP('',(#5363,#5364,#5365,#5366));
#1586=EDGE_LOOP('',(#5367,#5368,#5369,#5370));
#1587=EDGE_LOOP('',(#5371));
#1588=EDGE_LOOP('',(#5372,#5373,#5374,#5375));
#1589=EDGE_LOOP('',(#5376,#5377,#5378,#5379));
#1590=EDGE_LOOP('',(#5380,#5381,#5382,#5383));
#1591=EDGE_LOOP('',(#5384,#5385,#5386,#5387));
#1592=EDGE_LOOP('',(#5388,#5389,#5390,#5391));
#1593=EDGE_LOOP('',(#5392,#5393,#5394,#5395));
#1594=EDGE_LOOP('',(#5396));
#1595=EDGE_LOOP('',(#5397,#5398,#5399,#5400));
#1596=EDGE_LOOP('',(#5401,#5402,#5403,#5404));
#1597=EDGE_LOOP('',(#5405));
#1598=EDGE_LOOP('',(#5406,#5407,#5408,#5409));
#1599=EDGE_LOOP('',(#5410,#5411,#5412,#5413));
#1600=EDGE_LOOP('',(#5414,#5415));
#1601=EDGE_LOOP('',(#5416,#5417,#5418,#5419));
#1602=EDGE_LOOP('',(#5420));
#1603=EDGE_LOOP('',(#5421,#5422,#5423,#5424));
#1604=EDGE_LOOP('',(#5425,#5426,#5427,#5428));
#1605=EDGE_LOOP('',(#5429));
#1606=EDGE_LOOP('',(#5430));
#1607=EDGE_LOOP('',(#5431,#5432,#5433,#5434));
#1608=EDGE_LOOP('',(#5435,#5436,#5437,#5438));
#1609=EDGE_LOOP('',(#5439));
#1610=EDGE_LOOP('',(#5440));
#1611=EDGE_LOOP('',(#5441));
#1612=EDGE_LOOP('',(#5442));
#1613=EDGE_LOOP('',(#5443,#5444,#5445,#5446));
#1614=EDGE_LOOP('',(#5447));
#1615=EDGE_LOOP('',(#5448));
#1616=EDGE_LOOP('',(#5449,#5450,#5451,#5452));
#1617=EDGE_LOOP('',(#5453,#5454,#5455,#5456));
#1618=EDGE_LOOP('',(#5457));
#1619=EDGE_LOOP('',(#5458));
#1620=EDGE_LOOP('',(#5459));
#1621=EDGE_LOOP('',(#5460));
#1622=EDGE_LOOP('',(#5461,#5462,#5463,#5464,#5465,#5466,#5467,#5468));
#1623=EDGE_LOOP('',(#5469,#5470,#5471,#5472));
#1624=EDGE_LOOP('',(#5473,#5474,#5475,#5476));
#1625=EDGE_LOOP('',(#5477,#5478,#5479,#5480));
#1626=EDGE_LOOP('',(#5481,#5482,#5483,#5484));
#1627=EDGE_LOOP('',(#5485,#5486,#5487,#5488,#5489,#5490,#5491,#5492));
#1628=EDGE_LOOP('',(#5493,#5494,#5495,#5496));
#1629=EDGE_LOOP('',(#5497,#5498,#5499,#5500));
#1630=EDGE_LOOP('',(#5501,#5502,#5503,#5504));
#1631=EDGE_LOOP('',(#5505,#5506,#5507,#5508));
#1632=EDGE_LOOP('',(#5509,#5510,#5511,#5512));
#1633=EDGE_LOOP('',(#5513,#5514,#5515,#5516));
#1634=EDGE_LOOP('',(#5517,#5518,#5519,#5520));
#1635=EDGE_LOOP('',(#5521,#5522,#5523,#5524));
#1636=EDGE_LOOP('',(#5525,#5526,#5527,#5528));
#1637=EDGE_LOOP('',(#5529,#5530,#5531,#5532));
#1638=EDGE_LOOP('',(#5533,#5534,#5535,#5536,#5537,#5538));
#1639=EDGE_LOOP('',(#5539));
#1640=EDGE_LOOP('',(#5540,#5541,#5542,#5543,#5544,#5545));
#1641=EDGE_LOOP('',(#5546,#5547,#5548,#5549));
#1642=EDGE_LOOP('',(#5550,#5551,#5552,#5553));
#1643=EDGE_LOOP('',(#5554,#5555,#5556,#5557));
#1644=EDGE_LOOP('',(#5558));
#1645=EDGE_LOOP('',(#5559,#5560,#5561,#5562,#5563,#5564));
#1646=EDGE_LOOP('',(#5565,#5566,#5567,#5568,#5569));
#1647=EDGE_LOOP('',(#5570,#5571,#5572,#5573));
#1648=EDGE_LOOP('',(#5574,#5575,#5576,#5577));
#1649=EDGE_LOOP('',(#5578));
#1650=EDGE_LOOP('',(#5579));
#1651=EDGE_LOOP('',(#5580,#5581,#5582,#5583,#5584));
#1652=EDGE_LOOP('',(#5585));
#1653=EDGE_LOOP('',(#5586));
#1654=EDGE_LOOP('',(#5587,#5588,#5589,#5590));
#1655=EDGE_LOOP('',(#5591,#5592,#5593,#5594,#5595,#5596));
#1656=EDGE_LOOP('',(#5597,#5598,#5599,#5600,#5601));
#1657=EDGE_LOOP('',(#5602));
#1658=EDGE_LOOP('',(#5603));
#1659=EDGE_LOOP('',(#5604,#5605,#5606,#5607));
#1660=EDGE_LOOP('',(#5608,#5609,#5610,#5611));
#1661=EDGE_LOOP('',(#5612,#5613,#5614,#5615));
#1662=EDGE_LOOP('',(#5616));
#1663=EDGE_LOOP('',(#5617));
#1664=EDGE_LOOP('',(#5618,#5619,#5620,#5621,#5622));
#1665=EDGE_LOOP('',(#5623,#5624));
#1666=EDGE_LOOP('',(#5625,#5626));
#1667=EDGE_LOOP('',(#5627,#5628));
#1668=EDGE_LOOP('',(#5629,#5630));
#1669=EDGE_LOOP('',(#5631,#5632));
#1670=EDGE_LOOP('',(#5633,#5634));
#1671=EDGE_LOOP('',(#5635,#5636));
#1672=EDGE_LOOP('',(#5637,#5638));
#1673=EDGE_LOOP('',(#5639,#5640,#5641,#5642));
#1674=EDGE_LOOP('',(#5643,#5644,#5645,#5646,#5647,#5648,#5649,#5650,#5651,
#5652,#5653,#5654,#5655,#5656,#5657,#5658,#5659,#5660,#5661,#5662));
#1675=EDGE_LOOP('',(#5663,#5664,#5665,#5666));
#1676=EDGE_LOOP('',(#5667,#5668,#5669,#5670));
#1677=EDGE_LOOP('',(#5671,#5672,#5673,#5674));
#1678=EDGE_LOOP('',(#5675,#5676,#5677,#5678));
#1679=EDGE_LOOP('',(#5679,#5680,#5681,#5682));
#1680=EDGE_LOOP('',(#5683,#5684,#5685,#5686,#5687,#5688));
#1681=EDGE_LOOP('',(#5689,#5690,#5691,#5692));
#1682=EDGE_LOOP('',(#5693,#5694,#5695,#5696));
#1683=EDGE_LOOP('',(#5697,#5698,#5699,#5700));
#1684=EDGE_LOOP('',(#5701,#5702,#5703,#5704));
#1685=EDGE_LOOP('',(#5705,#5706,#5707,#5708));
#1686=EDGE_LOOP('',(#5709,#5710,#5711,#5712));
#1687=EDGE_LOOP('',(#5713,#5714,#5715,#5716,#5717,#5718,#5719,#5720,#5721,
#5722,#5723,#5724,#5725,#5726,#5727,#5728,#5729,#5730,#5731,#5732));
#1688=EDGE_LOOP('',(#5733,#5734,#5735,#5736));
#1689=EDGE_LOOP('',(#5737,#5738,#5739,#5740));
#1690=EDGE_LOOP('',(#5741));
#1691=EDGE_LOOP('',(#5742));
#1692=EDGE_LOOP('',(#5743,#5744,#5745,#5746));
#1693=EDGE_LOOP('',(#5747));
#1694=EDGE_LOOP('',(#5748));
#1695=EDGE_LOOP('',(#5749,#5750,#5751,#5752));
#1696=EDGE_LOOP('',(#5753));
#1697=EDGE_LOOP('',(#5754));
#1698=EDGE_LOOP('',(#5755,#5756,#5757,#5758));
#1699=EDGE_LOOP('',(#5759));
#1700=EDGE_LOOP('',(#5760));
#1701=EDGE_LOOP('',(#5761,#5762,#5763,#5764));
#1702=EDGE_LOOP('',(#5765));
#1703=EDGE_LOOP('',(#5766));
#1704=EDGE_LOOP('',(#5767,#5768,#5769,#5770));
#1705=EDGE_LOOP('',(#5771,#5772,#5773,#5774));
#1706=EDGE_LOOP('',(#5775,#5776,#5777,#5778));
#1707=EDGE_LOOP('',(#5779,#5780,#5781,#5782));
#1708=EDGE_LOOP('',(#5783,#5784,#5785,#5786));
#1709=EDGE_LOOP('',(#5787));
#1710=EDGE_LOOP('',(#5788,#5789,#5790,#5791));
#1711=EDGE_LOOP('',(#5792,#5793,#5794,#5795));
#1712=EDGE_LOOP('',(#5796));
#1713=EDGE_LOOP('',(#5797,#5798,#5799,#5800));
#1714=EDGE_LOOP('',(#5801));
#1715=EDGE_LOOP('',(#5802,#5803,#5804,#5805));
#1716=EDGE_LOOP('',(#5806));
#1717=EDGE_LOOP('',(#5807,#5808,#5809,#5810,#5811,#5812,#5813,#5814));
#1718=EDGE_LOOP('',(#5815,#5816,#5817,#5818));
#1719=EDGE_LOOP('',(#5819));
#1720=EDGE_LOOP('',(#5820,#5821,#5822,#5823,#5824,#5825,#5826,#5827));
#1721=EDGE_LOOP('',(#5828,#5829,#5830,#5831));
#1722=EDGE_LOOP('',(#5832,#5833,#5834,#5835));
#1723=EDGE_LOOP('',(#5836));
#1724=EDGE_LOOP('',(#5837,#5838,#5839,#5840));
#1725=EDGE_LOOP('',(#5841));
#1726=EDGE_LOOP('',(#5842,#5843,#5844,#5845));
#1727=EDGE_LOOP('',(#5846));
#1728=EDGE_LOOP('',(#5847,#5848,#5849,#5850));
#1729=EDGE_LOOP('',(#5851));
#1730=EDGE_LOOP('',(#5852));
#1731=EDGE_LOOP('',(#5853));
#1732=EDGE_LOOP('',(#5854));
#1733=EDGE_LOOP('',(#5855,#5856,#5857,#5858));
#1734=EDGE_LOOP('',(#5859,#5860,#5861,#5862));
#1735=EDGE_LOOP('',(#5863));
#1736=EDGE_LOOP('',(#5864));
#1737=EDGE_LOOP('',(#5865));
#1738=EDGE_LOOP('',(#5866));
#1739=EDGE_LOOP('',(#5867,#5868,#5869,#5870));
#1740=EDGE_LOOP('',(#5871,#5872,#5873,#5874));
#1741=EDGE_LOOP('',(#5875));
#1742=EDGE_LOOP('',(#5876));
#1743=EDGE_LOOP('',(#5877));
#1744=EDGE_LOOP('',(#5878));
#1745=EDGE_LOOP('',(#5879,#5880,#5881,#5882));
#1746=EDGE_LOOP('',(#5883,#5884,#5885,#5886));
#1747=EDGE_LOOP('',(#5887));
#1748=EDGE_LOOP('',(#5888));
#1749=EDGE_LOOP('',(#5889));
#1750=EDGE_LOOP('',(#5890));
#1751=EDGE_LOOP('',(#5891,#5892,#5893,#5894));
#1752=EDGE_LOOP('',(#5895,#5896,#5897,#5898));
#1753=EDGE_LOOP('',(#5899));
#1754=EDGE_LOOP('',(#5900));
#1755=EDGE_LOOP('',(#5901));
#1756=EDGE_LOOP('',(#5902));
#1757=EDGE_LOOP('',(#5903,#5904,#5905,#5906));
#1758=EDGE_LOOP('',(#5907,#5908,#5909,#5910));
#1759=EDGE_LOOP('',(#5911));
#1760=EDGE_LOOP('',(#5912));
#1761=EDGE_LOOP('',(#5913));
#1762=EDGE_LOOP('',(#5914));
#1763=EDGE_LOOP('',(#5915,#5916,#5917,#5918));
#1764=EDGE_LOOP('',(#5919,#5920,#5921,#5922));
#1765=EDGE_LOOP('',(#5923));
#1766=EDGE_LOOP('',(#5924));
#1767=EDGE_LOOP('',(#5925));
#1768=EDGE_LOOP('',(#5926));
#1769=EDGE_LOOP('',(#5927,#5928,#5929,#5930));
#1770=EDGE_LOOP('',(#5931,#5932,#5933,#5934));
#1771=EDGE_LOOP('',(#5935,#5936,#5937,#5938));
#1772=EDGE_LOOP('',(#5939,#5940,#5941,#5942));
#1773=EDGE_LOOP('',(#5943,#5944,#5945,#5946));
#1774=EDGE_LOOP('',(#5947,#5948,#5949,#5950));
#1775=EDGE_LOOP('',(#5951,#5952,#5953,#5954,#5955,#5956));
#1776=EDGE_LOOP('',(#5957,#5958,#5959,#5960,#5961,#5962));
#1777=EDGE_LOOP('',(#5963));
#1778=EDGE_LOOP('',(#5964));
#1779=EDGE_LOOP('',(#5965,#5966,#5967,#5968));
#1780=EDGE_LOOP('',(#5969,#5970,#5971,#5972));
#1781=EDGE_LOOP('',(#5973,#5974,#5975,#5976));
#1782=EDGE_LOOP('',(#5977));
#1783=EDGE_LOOP('',(#5978));
#1784=EDGE_LOOP('',(#5979,#5980,#5981,#5982));
#1785=EDGE_LOOP('',(#5983,#5984,#5985,#5986));
#1786=LINE('',#9932,#2201);
#1787=LINE('',#9938,#2202);
#1788=LINE('',#9944,#2203);
#1789=LINE('',#9950,#2204);
#1790=LINE('',#9955,#2205);
#1791=LINE('',#9957,#2206);
#1792=LINE('',#9959,#2207);
#1793=LINE('',#9960,#2208);
#1794=LINE('',#9963,#2209);
#1795=LINE('',#9965,#2210);
#1796=LINE('',#9966,#2211);
#1797=LINE('',#9969,#2212);
#1798=LINE('',#9971,#2213);
#1799=LINE('',#9972,#2214);
#1800=LINE('',#9974,#2215);
#1801=LINE('',#9975,#2216);
#1802=LINE('',#9983,#2217);
#1803=LINE('',#9990,#2218);
#1804=LINE('',#9997,#2219);
#1805=LINE('',#10004,#2220);
#1806=LINE('',#10011,#2221);
#1807=LINE('',#10018,#2222);
#1808=LINE('',#10025,#2223);
#1809=LINE('',#10032,#2224);
#1810=LINE('',#10038,#2225);
#1811=LINE('',#10042,#2226);
#1812=LINE('',#10047,#2227);
#1813=LINE('',#10051,#2228);
#1814=LINE('',#10054,#2229);
#1815=LINE('',#10055,#2230);
#1816=LINE('',#10061,#2231);
#1817=LINE('',#10065,#2232);
#1818=LINE('',#10070,#2233);
#1819=LINE('',#10074,#2234);
#1820=LINE('',#10077,#2235);
#1821=LINE('',#10078,#2236);
#1822=LINE('',#10084,#2237);
#1823=LINE('',#10088,#2238);
#1824=LINE('',#10093,#2239);
#1825=LINE('',#10097,#2240);
#1826=LINE('',#10100,#2241);
#1827=LINE('',#10101,#2242);
#1828=LINE('',#10107,#2243);
#1829=LINE('',#10111,#2244);
#1830=LINE('',#10116,#2245);
#1831=LINE('',#10120,#2246);
#1832=LINE('',#10123,#2247);
#1833=LINE('',#10124,#2248);
#1834=LINE('',#10129,#2249);
#1835=LINE('',#10131,#2250);
#1836=LINE('',#10132,#2251);
#1837=LINE('',#10135,#2252);
#1838=LINE('',#10137,#2253);
#1839=LINE('',#10138,#2254);
#1840=LINE('',#10141,#2255);
#1841=LINE('',#10143,#2256);
#1842=LINE('',#10144,#2257);
#1843=LINE('',#10147,#2258);
#1844=LINE('',#10149,#2259);
#1845=LINE('',#10150,#2260);
#1846=LINE('',#10153,#2261);
#1847=LINE('',#10155,#2262);
#1848=LINE('',#10157,#2263);
#1849=LINE('',#10158,#2264);
#1850=LINE('',#10160,#2265);
#1851=LINE('',#10164,#2266);
#1852=LINE('',#10165,#2267);
#1853=LINE('',#10168,#2268);
#1854=LINE('',#10169,#2269);
#1855=LINE('',#10173,#2270);
#1856=LINE('',#10175,#2271);
#1857=LINE('',#10177,#2272);
#1858=LINE('',#10179,#2273);
#1859=LINE('',#10180,#2274);
#1860=LINE('',#10183,#2275);
#1861=LINE('',#10184,#2276);
#1862=LINE('',#10187,#2277);
#1863=LINE('',#10188,#2278);
#1864=LINE('',#10192,#2279);
#1865=LINE('',#10196,#2280);
#1866=LINE('',#10200,#2281);
#1867=LINE('',#10204,#2282);
#1868=LINE('',#10207,#2283);
#1869=LINE('',#10208,#2284);
#1870=LINE('',#10211,#2285);
#1871=LINE('',#10212,#2286);
#1872=LINE('',#10214,#2287);
#1873=LINE('',#10219,#2288);
#1874=LINE('',#10220,#2289);
#1875=LINE('',#10223,#2290);
#1876=LINE('',#10224,#2291);
#1877=LINE('',#10226,#2292);
#1878=LINE('',#10233,#2293);
#1879=LINE('',#10239,#2294);
#1880=LINE('',#10248,#2295);
#1881=LINE('',#10254,#2296);
#1882=LINE('',#10263,#2297);
#1883=LINE('',#10269,#2298);
#1884=LINE('',#10275,#2299);
#1885=LINE('',#10281,#2300);
#1886=LINE('',#10287,#2301);
#1887=LINE('',#10294,#2302);
#1888=LINE('',#10300,#2303);
#1889=LINE('',#10309,#2304);
#1890=LINE('',#10315,#2305);
#1891=LINE('',#10321,#2306);
#1892=LINE('',#10327,#2307);
#1893=LINE('',#10333,#2308);
#1894=LINE('',#10341,#2309);
#1895=LINE('',#10346,#2310);
#1896=LINE('',#10354,#2311);
#1897=LINE('',#10356,#2312);
#1898=LINE('',#10358,#2313);
#1899=LINE('',#10359,#2314);
#1900=LINE('',#10362,#2315);
#1901=LINE('',#10364,#2316);
#1902=LINE('',#10365,#2317);
#1903=LINE('',#10368,#2318);
#1904=LINE('',#10370,#2319);
#1905=LINE('',#10371,#2320);
#1906=LINE('',#10373,#2321);
#1907=LINE('',#10374,#2322);
#1908=LINE('',#10381,#2323);
#1909=LINE('',#10383,#2324);
#1910=LINE('',#10385,#2325);
#1911=LINE('',#10386,#2326);
#1912=LINE('',#10389,#2327);
#1913=LINE('',#10391,#2328);
#1914=LINE('',#10392,#2329);
#1915=LINE('',#10395,#2330);
#1916=LINE('',#10397,#2331);
#1917=LINE('',#10398,#2332);
#1918=LINE('',#10400,#2333);
#1919=LINE('',#10401,#2334);
#1920=LINE('',#10418,#2335);
#1921=LINE('',#10424,#2336);
#1922=LINE('',#10428,#2337);
#1923=LINE('',#10434,#2338);
#1924=LINE('',#10439,#2339);
#1925=LINE('',#10454,#2340);
#1926=LINE('',#10463,#2341);
#1927=LINE('',#10467,#2342);
#1928=LINE('',#10471,#2343);
#1929=LINE('',#10474,#2344);
#1930=LINE('',#10643,#2345);
#1931=LINE('',#10979,#2346);
#1932=LINE('',#11021,#2347);
#1933=LINE('',#11026,#2348);
#1934=LINE('',#11035,#2349);
#1935=LINE('',#11040,#2350);
#1936=LINE('',#11053,#2351);
#1937=LINE('',#11057,#2352);
#1938=LINE('',#11061,#2353);
#1939=LINE('',#11068,#2354);
#1940=LINE('',#11072,#2355);
#1941=LINE('',#11076,#2356);
#1942=LINE('',#11081,#2357);
#1943=LINE('',#11083,#2358);
#1944=LINE('',#11085,#2359);
#1945=LINE('',#11086,#2360);
#1946=LINE('',#11089,#2361);
#1947=LINE('',#11091,#2362);
#1948=LINE('',#11092,#2363);
#1949=LINE('',#11095,#2364);
#1950=LINE('',#11097,#2365);
#1951=LINE('',#11098,#2366);
#1952=LINE('',#11101,#2367);
#1953=LINE('',#11103,#2368);
#1954=LINE('',#11104,#2369);
#1955=LINE('',#11107,#2370);
#1956=LINE('',#11109,#2371);
#1957=LINE('',#11110,#2372);
#1958=LINE('',#11112,#2373);
#1959=LINE('',#11113,#2374);
#1960=LINE('',#11123,#2375);
#1961=LINE('',#11127,#2376);
#1962=LINE('',#11131,#2377);
#1963=LINE('',#11138,#2378);
#1964=LINE('',#11142,#2379);
#1965=LINE('',#11146,#2380);
#1966=LINE('',#11151,#2381);
#1967=LINE('',#11153,#2382);
#1968=LINE('',#11155,#2383);
#1969=LINE('',#11156,#2384);
#1970=LINE('',#11159,#2385);
#1971=LINE('',#11161,#2386);
#1972=LINE('',#11162,#2387);
#1973=LINE('',#11165,#2388);
#1974=LINE('',#11167,#2389);
#1975=LINE('',#11168,#2390);
#1976=LINE('',#11171,#2391);
#1977=LINE('',#11173,#2392);
#1978=LINE('',#11174,#2393);
#1979=LINE('',#11177,#2394);
#1980=LINE('',#11179,#2395);
#1981=LINE('',#11180,#2396);
#1982=LINE('',#11182,#2397);
#1983=LINE('',#11183,#2398);
#1984=LINE('',#11212,#2399);
#1985=LINE('',#11214,#2400);
#1986=LINE('',#11216,#2401);
#1987=LINE('',#11217,#2402);
#1988=LINE('',#11222,#2403);
#1989=LINE('',#11223,#2404);
#1990=LINE('',#11226,#2405);
#1991=LINE('',#11228,#2406);
#1992=LINE('',#11229,#2407);
#1993=LINE('',#11231,#2408);
#1994=LINE('',#11237,#2409);
#1995=LINE('',#11239,#2410);
#1996=LINE('',#11241,#2411);
#1997=LINE('',#11242,#2412);
#1998=LINE('',#11247,#2413);
#1999=LINE('',#11248,#2414);
#2000=LINE('',#11251,#2415);
#2001=LINE('',#11253,#2416);
#2002=LINE('',#11254,#2417);
#2003=LINE('',#11256,#2418);
#2004=LINE('',#11270,#2419);
#2005=LINE('',#11273,#2420);
#2006=LINE('',#11278,#2421);
#2007=LINE('',#11286,#2422);
#2008=LINE('',#11292,#2423);
#2009=LINE('',#11300,#2424);
#2010=LINE('',#11321,#2425);
#2011=LINE('',#11376,#2426);
#2012=LINE('',#11381,#2427);
#2013=LINE('',#11387,#2428);
#2014=LINE('',#11395,#2429);
#2015=LINE('',#11416,#2430);
#2016=LINE('',#11471,#2431);
#2017=LINE('',#11475,#2432);
#2018=LINE('',#11477,#2433);
#2019=LINE('',#11479,#2434);
#2020=LINE('',#11480,#2435);
#2021=LINE('',#11483,#2436);
#2022=LINE('',#11485,#2437);
#2023=LINE('',#11487,#2438);
#2024=LINE('',#11489,#2439);
#2025=LINE('',#11490,#2440);
#2026=LINE('',#11493,#2441);
#2027=LINE('',#11495,#2442);
#2028=LINE('',#11497,#2443);
#2029=LINE('',#11499,#2444);
#2030=LINE('',#11500,#2445);
#2031=LINE('',#11502,#2446);
#2032=LINE('',#11503,#2447);
#2033=LINE('',#11512,#2448);
#2034=LINE('',#11514,#2449);
#2035=LINE('',#11516,#2450);
#2036=LINE('',#11517,#2451);
#2037=LINE('',#11520,#2452);
#2038=LINE('',#11522,#2453);
#2039=LINE('',#11523,#2454);
#2040=LINE('',#11526,#2455);
#2041=LINE('',#11528,#2456);
#2042=LINE('',#11529,#2457);
#2043=LINE('',#11531,#2458);
#2044=LINE('',#11532,#2459);
#2045=LINE('',#11541,#2460);
#2046=LINE('',#11546,#2461);
#2047=LINE('',#11567,#2462);
#2048=LINE('',#11622,#2463);
#2049=LINE('',#11626,#2464);
#2050=LINE('',#11628,#2465);
#2051=LINE('',#11630,#2466);
#2052=LINE('',#11631,#2467);
#2053=LINE('',#11634,#2468);
#2054=LINE('',#11636,#2469);
#2055=LINE('',#11637,#2470);
#2056=LINE('',#11640,#2471);
#2057=LINE('',#11642,#2472);
#2058=LINE('',#11643,#2473);
#2059=LINE('',#11654,#2474);
#2060=LINE('',#11659,#2475);
#2061=LINE('',#11663,#2476);
#2062=LINE('',#11667,#2477);
#2063=LINE('',#11670,#2478);
#2064=LINE('',#11673,#2479);
#2065=LINE('',#11674,#2480);
#2066=LINE('',#11677,#2481);
#2067=LINE('',#11680,#2482);
#2068=LINE('',#11683,#2483);
#2069=LINE('',#11691,#2484);
#2070=LINE('',#11698,#2485);
#2071=LINE('',#11704,#2486);
#2072=LINE('',#11713,#2487);
#2073=LINE('',#11721,#2488);
#2074=LINE('',#11726,#2489);
#2075=LINE('',#11734,#2490);
#2076=LINE('',#11736,#2491);
#2077=LINE('',#11738,#2492);
#2078=LINE('',#11740,#2493);
#2079=LINE('',#11742,#2494);
#2080=LINE('',#11744,#2495);
#2081=LINE('',#11746,#2496);
#2082=LINE('',#11747,#2497);
#2083=LINE('',#11750,#2498);
#2084=LINE('',#11752,#2499);
#2085=LINE('',#11753,#2500);
#2086=LINE('',#11756,#2501);
#2087=LINE('',#11757,#2502);
#2088=LINE('',#11760,#2503);
#2089=LINE('',#11761,#2504);
#2090=LINE('',#11764,#2505);
#2091=LINE('',#11765,#2506);
#2092=LINE('',#11768,#2507);
#2093=LINE('',#11770,#2508);
#2094=LINE('',#11772,#2509);
#2095=LINE('',#11773,#2510);
#2096=LINE('',#11775,#2511);
#2097=LINE('',#11777,#2512);
#2098=LINE('',#11779,#2513);
#2099=LINE('',#11785,#2514);
#2100=LINE('',#11787,#2515);
#2101=LINE('',#11789,#2516);
#2102=LINE('',#11790,#2517);
#2103=LINE('',#11793,#2518);
#2104=LINE('',#11795,#2519);
#2105=LINE('',#11796,#2520);
#2106=LINE('',#11799,#2521);
#2107=LINE('',#11801,#2522);
#2108=LINE('',#11802,#2523);
#2109=LINE('',#11805,#2524);
#2110=LINE('',#11807,#2525);
#2111=LINE('',#11808,#2526);
#2112=LINE('',#11811,#2527);
#2113=LINE('',#11813,#2528);
#2114=LINE('',#11814,#2529);
#2115=LINE('',#11816,#2530);
#2116=LINE('',#11817,#2531);
#2117=LINE('',#11825,#2532);
#2118=LINE('',#11829,#2533);
#2119=LINE('',#11833,#2534);
#2120=LINE('',#11849,#2535);
#2121=LINE('',#11855,#2536);
#2122=LINE('',#11859,#2537);
#2123=LINE('',#11865,#2538);
#2124=LINE('',#11870,#2539);
#2125=LINE('',#11885,#2540);
#2126=LINE('',#11894,#2541);
#2127=LINE('',#11898,#2542);
#2128=LINE('',#11902,#2543);
#2129=LINE('',#11905,#2544);
#2130=LINE('',#12058,#2545);
#2131=LINE('',#12354,#2546);
#2132=LINE('',#12396,#2547);
#2133=LINE('',#12401,#2548);
#2134=LINE('',#12410,#2549);
#2135=LINE('',#12415,#2550);
#2136=LINE('',#12440,#2551);
#2137=LINE('',#12446,#2552);
#2138=LINE('',#12452,#2553);
#2139=LINE('',#12457,#2554);
#2140=LINE('',#12459,#2555);
#2141=LINE('',#12461,#2556);
#2142=LINE('',#12462,#2557);
#2143=LINE('',#12466,#2558);
#2144=LINE('',#12468,#2559);
#2145=LINE('',#12470,#2560);
#2146=LINE('',#12471,#2561);
#2147=LINE('',#12474,#2562);
#2148=LINE('',#12476,#2563);
#2149=LINE('',#12477,#2564);
#2150=LINE('',#12479,#2565);
#2151=LINE('',#12480,#2566);
#2152=LINE('',#12483,#2567);
#2153=LINE('',#12485,#2568);
#2154=LINE('',#12486,#2569);
#2155=LINE('',#12490,#2570);
#2156=LINE('',#12491,#2571);
#2157=LINE('',#12492,#2572);
#2158=LINE('',#12495,#2573);
#2159=LINE('',#12496,#2574);
#2160=LINE('',#12499,#2575);
#2161=LINE('',#12500,#2576);
#2162=LINE('',#12502,#2577);
#2163=LINE('',#12509,#2578);
#2164=LINE('',#12516,#2579);
#2165=LINE('',#12523,#2580);
#2166=LINE('',#12532,#2581);
#2167=LINE('',#12538,#2582);
#2168=LINE('',#12547,#2583);
#2169=LINE('',#12553,#2584);
#2170=LINE('',#12562,#2585);
#2171=LINE('',#12568,#2586);
#2172=LINE('',#12577,#2587);
#2173=LINE('',#12583,#2588);
#2174=LINE('',#12592,#2589);
#2175=LINE('',#12598,#2590);
#2176=LINE('',#12607,#2591);
#2177=LINE('',#12613,#2592);
#2178=LINE('',#12621,#2593);
#2179=LINE('',#12623,#2594);
#2180=LINE('',#12625,#2595);
#2181=LINE('',#12626,#2596);
#2182=LINE('',#12629,#2597);
#2183=LINE('',#12631,#2598);
#2184=LINE('',#12632,#2599);
#2185=LINE('',#12635,#2600);
#2186=LINE('',#12637,#2601);
#2187=LINE('',#12638,#2602);
#2188=LINE('',#12641,#2603);
#2189=LINE('',#12643,#2604);
#2190=LINE('',#12644,#2605);
#2191=LINE('',#12647,#2606);
#2192=LINE('',#12649,#2607);
#2193=LINE('',#12650,#2608);
#2194=LINE('',#12652,#2609);
#2195=LINE('',#12653,#2610);
#2196=LINE('',#12665,#2611);
#2197=LINE('',#12669,#2612);
#2198=LINE('',#12673,#2613);
#2199=LINE('',#12680,#2614);
#2200=LINE('',#12682,#2615);
#2201=VECTOR('',#7820,0.25);
#2202=VECTOR('',#7827,0.25);
#2203=VECTOR('',#7834,0.25);
#2204=VECTOR('',#7841,0.25);
#2205=VECTOR('',#7846,1.);
#2206=VECTOR('',#7847,1.);
#2207=VECTOR('',#7848,1.);
#2208=VECTOR('',#7849,1.);
#2209=VECTOR('',#7852,1.);
#2210=VECTOR('',#7853,1.);
#2211=VECTOR('',#7854,1.);
#2212=VECTOR('',#7857,1.);
#2213=VECTOR('',#7858,1.);
#2214=VECTOR('',#7859,1.);
#2215=VECTOR('',#7862,1.);
#2216=VECTOR('',#7863,1.);
#2217=VECTOR('',#7874,0.165);
#2218=VECTOR('',#7883,0.165);
#2219=VECTOR('',#7892,0.165);
#2220=VECTOR('',#7901,0.165);
#2221=VECTOR('',#7910,0.165);
#2222=VECTOR('',#7919,0.165);
#2223=VECTOR('',#7928,0.165);
#2224=VECTOR('',#7937,0.165);
#2225=VECTOR('',#7944,1.);
#2226=VECTOR('',#7947,1.);
#2227=VECTOR('',#7952,1.);
#2228=VECTOR('',#7955,1.);
#2229=VECTOR('',#7960,1.);
#2230=VECTOR('',#7961,1.);
#2231=VECTOR('',#7966,1.);
#2232=VECTOR('',#7969,1.);
#2233=VECTOR('',#7974,1.);
#2234=VECTOR('',#7977,1.);
#2235=VECTOR('',#7982,1.);
#2236=VECTOR('',#7983,1.);
#2237=VECTOR('',#7988,1.);
#2238=VECTOR('',#7991,1.);
#2239=VECTOR('',#7996,1.);
#2240=VECTOR('',#7999,1.);
#2241=VECTOR('',#8004,1.);
#2242=VECTOR('',#8005,1.);
#2243=VECTOR('',#8010,1.);
#2244=VECTOR('',#8013,1.);
#2245=VECTOR('',#8018,1.);
#2246=VECTOR('',#8021,1.);
#2247=VECTOR('',#8026,1.);
#2248=VECTOR('',#8027,1.);
#2249=VECTOR('',#8032,1.);
#2250=VECTOR('',#8033,1.);
#2251=VECTOR('',#8034,1.);
#2252=VECTOR('',#8037,1.);
#2253=VECTOR('',#8038,1.);
#2254=VECTOR('',#8039,1.);
#2255=VECTOR('',#8042,1.);
#2256=VECTOR('',#8043,1.);
#2257=VECTOR('',#8044,1.);
#2258=VECTOR('',#8047,1.);
#2259=VECTOR('',#8048,1.);
#2260=VECTOR('',#8049,1.);
#2261=VECTOR('',#8052,1.);
#2262=VECTOR('',#8053,1.);
#2263=VECTOR('',#8054,1.);
#2264=VECTOR('',#8055,1.);
#2265=VECTOR('',#8056,1.);
#2266=VECTOR('',#8061,1.);
#2267=VECTOR('',#8062,1.);
#2268=VECTOR('',#8065,1.);
#2269=VECTOR('',#8066,1.);
#2270=VECTOR('',#8071,1.);
#2271=VECTOR('',#8072,1.);
#2272=VECTOR('',#8073,1.);
#2273=VECTOR('',#8074,1.);
#2274=VECTOR('',#8075,1.);
#2275=VECTOR('',#8078,1.);
#2276=VECTOR('',#8079,1.);
#2277=VECTOR('',#8082,1.);
#2278=VECTOR('',#8083,1.);
#2279=VECTOR('',#8088,0.33);
#2280=VECTOR('',#8093,0.33);
#2281=VECTOR('',#8098,0.33);
#2282=VECTOR('',#8103,0.33);
#2283=VECTOR('',#8106,1.);
#2284=VECTOR('',#8107,1.);
#2285=VECTOR('',#8110,1.);
#2286=VECTOR('',#8111,1.);
#2287=VECTOR('',#8114,1.);
#2288=VECTOR('',#8121,1.);
#2289=VECTOR('',#8122,1.);
#2290=VECTOR('',#8125,1.);
#2291=VECTOR('',#8126,1.);
#2292=VECTOR('',#8129,1.);
#2293=VECTOR('',#8138,2.6);
#2294=VECTOR('',#8145,4.);
#2295=VECTOR('',#8158,2.);
#2296=VECTOR('',#8165,2.59);
#2297=VECTOR('',#8178,0.225);
#2298=VECTOR('',#8185,0.225);
#2299=VECTOR('',#8192,0.225);
#2300=VECTOR('',#8199,0.225);
#2301=VECTOR('',#8206,2.59);
#2302=VECTOR('',#8215,2.);
#2303=VECTOR('',#8222,4.);
#2304=VECTOR('',#8235,0.225);
#2305=VECTOR('',#8242,0.225);
#2306=VECTOR('',#8249,0.225);
#2307=VECTOR('',#8256,0.225);
#2308=VECTOR('',#8263,2.59);
#2309=VECTOR('',#8274,2.);
#2310=VECTOR('',#8279,4.);
#2311=VECTOR('',#8290,1.);
#2312=VECTOR('',#8291,1.);
#2313=VECTOR('',#8292,1.);
#2314=VECTOR('',#8293,1.);
#2315=VECTOR('',#8296,1.);
#2316=VECTOR('',#8297,1.);
#2317=VECTOR('',#8298,1.);
#2318=VECTOR('',#8301,1.);
#2319=VECTOR('',#8302,1.);
#2320=VECTOR('',#8303,1.);
#2321=VECTOR('',#8306,1.);
#2322=VECTOR('',#8307,1.);
#2323=VECTOR('',#8316,1.);
#2324=VECTOR('',#8317,1.);
#2325=VECTOR('',#8318,1.);
#2326=VECTOR('',#8319,1.);
#2327=VECTOR('',#8322,1.);
#2328=VECTOR('',#8323,1.);
#2329=VECTOR('',#8324,1.);
#2330=VECTOR('',#8327,1.);
#2331=VECTOR('',#8328,1.);
#2332=VECTOR('',#8329,1.);
#2333=VECTOR('',#8332,1.);
#2334=VECTOR('',#8333,1.);
#2335=VECTOR('',#8356,1.88531);
#2336=VECTOR('',#8363,1.25);
#2337=VECTOR('',#8368,1.3);
#2338=VECTOR('',#8377,1.88531);
#2339=VECTOR('',#8384,1.3);
#2340=VECTOR('',#8403,1.96469);
#2341=VECTOR('',#8414,2.55);
#2342=VECTOR('',#8419,2.6);
#2343=VECTOR('',#8424,2.55);
#2344=VECTOR('',#8429,1.96469);
#2345=VECTOR('',#8486,1.956752);
#2346=VECTOR('',#8577,1.893248);
#2347=VECTOR('',#8606,1.95469);
#2348=VECTOR('',#8613,1.90031);
#2349=VECTOR('',#8624,1.95469);
#2350=VECTOR('',#8631,1.90031);
#2351=VECTOR('',#8652,0.475);
#2352=VECTOR('',#8657,0.5);
#2353=VECTOR('',#8662,0.485);
#2354=VECTOR('',#8671,0.31);
#2355=VECTOR('',#8676,0.3);
#2356=VECTOR('',#8681,0.27);
#2357=VECTOR('',#8686,1.);
#2358=VECTOR('',#8687,1.);
#2359=VECTOR('',#8688,1.);
#2360=VECTOR('',#8689,1.);
#2361=VECTOR('',#8692,1.);
#2362=VECTOR('',#8693,1.);
#2363=VECTOR('',#8694,1.);
#2364=VECTOR('',#8697,1.);
#2365=VECTOR('',#8698,1.);
#2366=VECTOR('',#8699,1.);
#2367=VECTOR('',#8702,1.);
#2368=VECTOR('',#8703,1.);
#2369=VECTOR('',#8704,1.);
#2370=VECTOR('',#8707,1.);
#2371=VECTOR('',#8708,1.);
#2372=VECTOR('',#8709,1.);
#2373=VECTOR('',#8712,1.);
#2374=VECTOR('',#8713,1.);
#2375=VECTOR('',#8728,0.325);
#2376=VECTOR('',#8733,0.35);
#2377=VECTOR('',#8738,0.335);
#2378=VECTOR('',#8747,0.21);
#2379=VECTOR('',#8752,0.2);
#2380=VECTOR('',#8757,0.18);
#2381=VECTOR('',#8762,1.);
#2382=VECTOR('',#8763,1.);
#2383=VECTOR('',#8764,1.);
#2384=VECTOR('',#8765,1.);
#2385=VECTOR('',#8768,1.);
#2386=VECTOR('',#8769,1.);
#2387=VECTOR('',#8770,1.);
#2388=VECTOR('',#8773,1.);
#2389=VECTOR('',#8774,1.);
#2390=VECTOR('',#8775,1.);
#2391=VECTOR('',#8778,1.);
#2392=VECTOR('',#8779,1.);
#2393=VECTOR('',#8780,1.);
#2394=VECTOR('',#8783,1.);
#2395=VECTOR('',#8784,1.);
#2396=VECTOR('',#8785,1.);
#2397=VECTOR('',#8788,1.);
#2398=VECTOR('',#8789,1.);
#2399=VECTOR('',#8842,1.);
#2400=VECTOR('',#8843,1.);
#2401=VECTOR('',#8844,1.);
#2402=VECTOR('',#8845,1.);
#2403=VECTOR('',#8850,1.);
#2404=VECTOR('',#8851,1.);
#2405=VECTOR('',#8854,1.);
#2406=VECTOR('',#8855,1.);
#2407=VECTOR('',#8856,1.);
#2408=VECTOR('',#8859,1.);
#2409=VECTOR('',#8866,1.);
#2410=VECTOR('',#8867,1.);
#2411=VECTOR('',#8868,1.);
#2412=VECTOR('',#8869,1.);
#2413=VECTOR('',#8874,1.);
#2414=VECTOR('',#8875,1.);
#2415=VECTOR('',#8878,1.);
#2416=VECTOR('',#8879,1.);
#2417=VECTOR('',#8880,1.);
#2418=VECTOR('',#8883,1.);
#2419=VECTOR('',#8902,1.6);
#2420=VECTOR('',#8905,1.25);
#2421=VECTOR('',#8912,1.25);
#2422=VECTOR('',#8923,1.255);
#2423=VECTOR('',#8930,1.7);
#2424=VECTOR('',#8941,1.);
#2425=VECTOR('',#8948,0.21);
#2426=VECTOR('',#8953,1.);
#2427=VECTOR('',#8958,1.255);
#2428=VECTOR('',#8965,1.8);
#2429=VECTOR('',#8976,1.);
#2430=VECTOR('',#8983,0.21);
#2431=VECTOR('',#8988,1.);
#2432=VECTOR('',#8991,1.);
#2433=VECTOR('',#8992,1.);
#2434=VECTOR('',#8993,1.);
#2435=VECTOR('',#8994,1.);
#2436=VECTOR('',#8997,1.);
#2437=VECTOR('',#8998,1.);
#2438=VECTOR('',#8999,1.);
#2439=VECTOR('',#9000,1.);
#2440=VECTOR('',#9001,1.);
#2441=VECTOR('',#9004,1.);
#2442=VECTOR('',#9005,1.);
#2443=VECTOR('',#9006,1.);
#2444=VECTOR('',#9007,1.);
#2445=VECTOR('',#9008,1.);
#2446=VECTOR('',#9011,1.);
#2447=VECTOR('',#9012,1.);
#2448=VECTOR('',#9023,1.);
#2449=VECTOR('',#9024,1.);
#2450=VECTOR('',#9025,1.);
#2451=VECTOR('',#9026,1.);
#2452=VECTOR('',#9029,1.);
#2453=VECTOR('',#9030,1.);
#2454=VECTOR('',#9031,1.);
#2455=VECTOR('',#9034,1.);
#2456=VECTOR('',#9035,1.);
#2457=VECTOR('',#9036,1.);
#2458=VECTOR('',#9039,1.);
#2459=VECTOR('',#9040,1.);
#2460=VECTOR('',#9055,2.);
#2461=VECTOR('',#9060,1.);
#2462=VECTOR('',#9067,0.21);
#2463=VECTOR('',#9072,1.);
#2464=VECTOR('',#9075,1.);
#2465=VECTOR('',#9076,1.);
#2466=VECTOR('',#9077,1.);
#2467=VECTOR('',#9078,1.);
#2468=VECTOR('',#9081,1.);
#2469=VECTOR('',#9082,1.);
#2470=VECTOR('',#9083,1.);
#2471=VECTOR('',#9086,1.);
#2472=VECTOR('',#9087,1.);
#2473=VECTOR('',#9088,1.);
#2474=VECTOR('',#9103,1.5);
#2475=VECTOR('',#9108,1.);
#2476=VECTOR('',#9111,1.);
#2477=VECTOR('',#9116,1.);
#2478=VECTOR('',#9119,1.);
#2479=VECTOR('',#9122,1.);
#2480=VECTOR('',#9123,1.);
#2481=VECTOR('',#9126,1.);
#2482=VECTOR('',#9131,1.);
#2483=VECTOR('',#9134,2.5);
#2484=VECTOR('',#9145,1.5);
#2485=VECTOR('',#9154,1.1);
#2486=VECTOR('',#9161,2.);
#2487=VECTOR('',#9174,1.5);
#2488=VECTOR('',#9185,1.1);
#2489=VECTOR('',#9190,2.);
#2490=VECTOR('',#9201,1.);
#2491=VECTOR('',#9202,1.);
#2492=VECTOR('',#9203,1.);
#2493=VECTOR('',#9204,1.);
#2494=VECTOR('',#9205,1.);
#2495=VECTOR('',#9206,1.);
#2496=VECTOR('',#9207,1.);
#2497=VECTOR('',#9208,1.);
#2498=VECTOR('',#9211,1.);
#2499=VECTOR('',#9212,1.);
#2500=VECTOR('',#9213,1.);
#2501=VECTOR('',#9216,1.);
#2502=VECTOR('',#9217,1.);
#2503=VECTOR('',#9220,1.);
#2504=VECTOR('',#9221,1.);
#2505=VECTOR('',#9224,1.);
#2506=VECTOR('',#9225,1.);
#2507=VECTOR('',#9228,1.);
#2508=VECTOR('',#9229,1.);
#2509=VECTOR('',#9230,1.);
#2510=VECTOR('',#9231,1.);
#2511=VECTOR('',#9234,1.);
#2512=VECTOR('',#9237,1.);
#2513=VECTOR('',#9240,1.);
#2514=VECTOR('',#9247,1.);
#2515=VECTOR('',#9248,1.);
#2516=VECTOR('',#9249,1.);
#2517=VECTOR('',#9250,1.);
#2518=VECTOR('',#9253,1.);
#2519=VECTOR('',#9254,1.);
#2520=VECTOR('',#9255,1.);
#2521=VECTOR('',#9258,1.);
#2522=VECTOR('',#9259,1.);
#2523=VECTOR('',#9260,1.);
#2524=VECTOR('',#9263,1.);
#2525=VECTOR('',#9264,1.);
#2526=VECTOR('',#9265,1.);
#2527=VECTOR('',#9268,1.);
#2528=VECTOR('',#9269,1.);
#2529=VECTOR('',#9270,1.);
#2530=VECTOR('',#9273,1.);
#2531=VECTOR('',#9274,1.);
#2532=VECTOR('',#9285,0.235);
#2533=VECTOR('',#9290,0.25);
#2534=VECTOR('',#9295,0.2125);
#2535=VECTOR('',#9316,0.976185);
#2536=VECTOR('',#9323,0.5);
#2537=VECTOR('',#9328,0.53);
#2538=VECTOR('',#9337,0.976185);
#2539=VECTOR('',#9344,0.53);
#2540=VECTOR('',#9363,1.023815);
#2541=VECTOR('',#9374,1.47);
#2542=VECTOR('',#9379,1.5);
#2543=VECTOR('',#9384,1.47);
#2544=VECTOR('',#9389,1.023815);
#2545=VECTOR('',#9440,1.019052);
#2546=VECTOR('',#9517,0.980948);
#2547=VECTOR('',#9546,1.013815);
#2548=VECTOR('',#9553,0.991185);
#2549=VECTOR('',#9564,1.013815);
#2550=VECTOR('',#9571,0.991185);
#2551=VECTOR('',#9616,0.329999999999998);
#2552=VECTOR('',#9623,0.505000000000003);
#2553=VECTOR('',#9630,0.505000000000003);
#2554=VECTOR('',#9635,1.);
#2555=VECTOR('',#9636,1.);
#2556=VECTOR('',#9637,1.);
#2557=VECTOR('',#9638,1.);
#2558=VECTOR('',#9641,1.);
#2559=VECTOR('',#9642,1.);
#2560=VECTOR('',#9643,1.);
#2561=VECTOR('',#9644,1.);
#2562=VECTOR('',#9647,1.);
#2563=VECTOR('',#9648,1.);
#2564=VECTOR('',#9649,1.);
#2565=VECTOR('',#9652,1.);
#2566=VECTOR('',#9653,1.);
#2567=VECTOR('',#9656,1.);
#2568=VECTOR('',#9657,1.);
#2569=VECTOR('',#9658,1.);
#2570=VECTOR('',#9661,1.);
#2571=VECTOR('',#9662,1.);
#2572=VECTOR('',#9663,1.);
#2573=VECTOR('',#9666,1.);
#2574=VECTOR('',#9667,1.);
#2575=VECTOR('',#9670,1.);
#2576=VECTOR('',#9671,1.);
#2577=VECTOR('',#9674,1.);
#2578=VECTOR('',#9683,0.164999999999999);
#2579=VECTOR('',#9692,0.164999999999999);
#2580=VECTOR('',#9701,0.5);
#2581=VECTOR('',#9714,0.505000000000003);
#2582=VECTOR('',#9721,0.700000000000003);
#2583=VECTOR('',#9734,0.505000000000003);
#2584=VECTOR('',#9741,0.700000000000003);
#2585=VECTOR('',#9754,0.505000000000003);
#2586=VECTOR('',#9761,0.700000000000003);
#2587=VECTOR('',#9774,0.505000000000003);
#2588=VECTOR('',#9781,0.700000000000003);
#2589=VECTOR('',#9794,0.225000000000001);
#2590=VECTOR('',#9801,0.799999999999997);
#2591=VECTOR('',#9814,0.225000000000001);
#2592=VECTOR('',#9821,0.799999999999997);
#2593=VECTOR('',#9832,1.);
#2594=VECTOR('',#9833,1.);
#2595=VECTOR('',#9834,1.);
#2596=VECTOR('',#9835,1.);
#2597=VECTOR('',#9838,1.);
#2598=VECTOR('',#9839,1.);
#2599=VECTOR('',#9840,1.);
#2600=VECTOR('',#9843,1.);
#2601=VECTOR('',#9844,1.);
#2602=VECTOR('',#9845,1.);
#2603=VECTOR('',#9848,1.);
#2604=VECTOR('',#9849,1.);
#2605=VECTOR('',#9850,1.);
#2606=VECTOR('',#9853,1.);
#2607=VECTOR('',#9854,1.);
#2608=VECTOR('',#9855,1.);
#2609=VECTOR('',#9858,1.);
#2610=VECTOR('',#9859,1.);
#2611=VECTOR('',#9876,0.325);
#2612=VECTOR('',#9881,0.35);
#2613=VECTOR('',#9886,0.335);
#2614=VECTOR('',#9895,0.21);
#2615=VECTOR('',#9898,0.2);
#2616=CIRCLE('',#6964,0.25);
#2617=CIRCLE('',#6965,0.25);
#2618=CIRCLE('',#6967,0.25);
#2619=CIRCLE('',#6968,0.25);
#2620=CIRCLE('',#6970,0.25);
#2621=CIRCLE('',#6971,0.25);
#2622=CIRCLE('',#6973,0.25);
#2623=CIRCLE('',#6974,0.25);
#2624=CIRCLE('',#6983,0.165);
#2625=CIRCLE('',#6984,0.165);
#2626=CIRCLE('',#6987,0.165);
#2627=CIRCLE('',#6988,0.165);
#2628=CIRCLE('',#6991,0.165);
#2629=CIRCLE('',#6992,0.165);
#2630=CIRCLE('',#6995,0.165);
#2631=CIRCLE('',#6996,0.165);
#2632=CIRCLE('',#6999,0.165);
#2633=CIRCLE('',#7000,0.165);
#2634=CIRCLE('',#7003,0.165);
#2635=CIRCLE('',#7004,0.165);
#2636=CIRCLE('',#7007,0.165);
#2637=CIRCLE('',#7008,0.165);
#2638=CIRCLE('',#7011,0.165);
#2639=CIRCLE('',#7012,0.165);
#2640=CIRCLE('',#7015,0.6);
#2641=CIRCLE('',#7016,0.6);
#2642=CIRCLE('',#7018,0.6);
#2643=CIRCLE('',#7019,0.6);
#2644=CIRCLE('',#7021,0.33);
#2645=CIRCLE('',#7023,0.6);
#2646=CIRCLE('',#7024,0.6);
#2647=CIRCLE('',#7026,0.6);
#2648=CIRCLE('',#7027,0.6);
#2649=CIRCLE('',#7029,0.33);
#2650=CIRCLE('',#7031,0.6);
#2651=CIRCLE('',#7032,0.6);
#2652=CIRCLE('',#7034,0.6);
#2653=CIRCLE('',#7035,0.6);
#2654=CIRCLE('',#7037,0.33);
#2655=CIRCLE('',#7039,0.6);
#2656=CIRCLE('',#7040,0.6);
#2657=CIRCLE('',#7042,0.6);
#2658=CIRCLE('',#7043,0.6);
#2659=CIRCLE('',#7045,0.33);
#2660=CIRCLE('',#7051,4.);
#2661=CIRCLE('',#7055,4.);
#2662=CIRCLE('',#7059,0.33);
#2663=CIRCLE('',#7061,0.33);
#2664=CIRCLE('',#7063,0.33);
#2665=CIRCLE('',#7065,0.33);
#2666=CIRCLE('',#7070,4.);
#2667=CIRCLE('',#7075,4.);
#2668=CIRCLE('',#7077,2.6);
#2669=CIRCLE('',#7078,2.6);
#2670=CIRCLE('',#7080,4.);
#2671=CIRCLE('',#7081,4.);
#2672=CIRCLE('',#7086,2.);
#2673=CIRCLE('',#7087,2.);
#2674=CIRCLE('',#7089,2.59);
#2675=CIRCLE('',#7090,2.59);
#2676=CIRCLE('',#7095,0.225);
#2677=CIRCLE('',#7096,0.225);
#2678=CIRCLE('',#7098,0.225);
#2679=CIRCLE('',#7099,0.225);
#2680=CIRCLE('',#7101,0.225);
#2681=CIRCLE('',#7102,0.225);
#2682=CIRCLE('',#7104,0.225);
#2683=CIRCLE('',#7105,0.225);
#2684=CIRCLE('',#7107,2.59);
#2685=CIRCLE('',#7108,2.59);
#2686=CIRCLE('',#7110,2.);
#2687=CIRCLE('',#7112,2.);
#2688=CIRCLE('',#7114,4.);
#2689=CIRCLE('',#7115,4.);
#2690=CIRCLE('',#7120,0.225);
#2691=CIRCLE('',#7121,0.225);
#2692=CIRCLE('',#7123,0.225);
#2693=CIRCLE('',#7124,0.225);
#2694=CIRCLE('',#7126,0.225);
#2695=CIRCLE('',#7127,0.225);
#2696=CIRCLE('',#7129,0.225);
#2697=CIRCLE('',#7130,0.225);
#2698=CIRCLE('',#7132,2.59);
#2699=CIRCLE('',#7133,2.59);
#2700=CIRCLE('',#7135,2.);
#2701=CIRCLE('',#7137,2.);
#2702=CIRCLE('',#7139,4.);
#2703=CIRCLE('',#7140,4.);
#2704=CIRCLE('',#7160,1.88531);
#2705=CIRCLE('',#7161,1.88531);
#2706=CIRCLE('',#7162,0.412776);
#2707=CIRCLE('',#7163,1.88531);
#2708=CIRCLE('',#7164,1.88531);
#2709=CIRCLE('',#7166,1.88531);
#2710=CIRCLE('',#7168,1.25);
#2711=CIRCLE('',#7169,1.25);
#2712=CIRCLE('',#7171,1.35);
#2713=CIRCLE('',#7174,1.88531);
#2714=CIRCLE('',#7176,1.35);
#2715=CIRCLE('',#7180,1.96469);
#2716=CIRCLE('',#7181,1.96469);
#2717=CIRCLE('',#7182,0.412776);
#2718=CIRCLE('',#7183,1.96469);
#2719=CIRCLE('',#7184,1.96469);
#2720=CIRCLE('',#7186,1.96469);
#2721=CIRCLE('',#7188,2.5);
#2722=CIRCLE('',#7189,1.96469);
#2723=CIRCLE('',#7191,2.6);
#2724=CIRCLE('',#7193,2.6);
#2725=CIRCLE('',#7195,2.5);
#2726=CIRCLE('',#7200,0.3969);
#2727=CIRCLE('',#7202,0.3969);
#2728=CIRCLE('',#7204,0.3969);
#2729=CIRCLE('',#7206,0.3969);
#2730=CIRCLE('',#7208,0.3969);
#2731=CIRCLE('',#7210,0.3969);
#2732=CIRCLE('',#7212,0.3969);
#2733=CIRCLE('',#7214,0.3969);
#2734=CIRCLE('',#7216,0.3969);
#2735=CIRCLE('',#7219,0.405071403305639);
#2736=CIRCLE('',#7220,0.405071403305639);
#2737=CIRCLE('',#7222,1.956752);
#2738=CIRCLE('',#7223,1.956752);
#2739=CIRCLE('',#7224,1.956752);
#2740=CIRCLE('',#7225,1.956752);
#2741=CIRCLE('',#7226,1.956752);
#2742=CIRCLE('',#7227,1.956752);
#2743=CIRCLE('',#7228,1.956752);
#2744=CIRCLE('',#7229,1.956752);
#2745=CIRCLE('',#7230,1.956752);
#2746=CIRCLE('',#7231,1.956752);
#2747=CIRCLE('',#7232,1.956752);
#2748=CIRCLE('',#7234,1.893248);
#2749=CIRCLE('',#7235,0.405071403305639);
#2750=CIRCLE('',#7237,0.405071403305639);
#2751=CIRCLE('',#7239,1.893248);
#2752=CIRCLE('',#7240,0.405071403305639);
#2753=CIRCLE('',#7242,0.405071403305639);
#2754=CIRCLE('',#7244,1.893248);
#2755=CIRCLE('',#7245,0.405071403305639);
#2756=CIRCLE('',#7247,0.405071403305639);
#2757=CIRCLE('',#7249,1.893248);
#2758=CIRCLE('',#7250,1.893248);
#2759=CIRCLE('',#7251,0.405071403305639);
#2760=CIRCLE('',#7253,0.405071403305639);
#2761=CIRCLE('',#7255,1.893248);
#2762=CIRCLE('',#7256,0.405071403305639);
#2763=CIRCLE('',#7258,0.405071403305639);
#2764=CIRCLE('',#7260,1.893248);
#2765=CIRCLE('',#7261,0.405071403305639);
#2766=CIRCLE('',#7263,0.405071403305639);
#2767=CIRCLE('',#7265,1.893248);
#2768=CIRCLE('',#7266,0.405071403305639);
#2769=CIRCLE('',#7268,0.405071403305639);
#2770=CIRCLE('',#7270,1.893248);
#2771=CIRCLE('',#7271,1.893248);
#2772=CIRCLE('',#7272,1.893248);
#2773=CIRCLE('',#7274,0.405071403305639);
#2774=CIRCLE('',#7276,0.405071403305639);
#2775=CIRCLE('',#7281,1.95469);
#2776=CIRCLE('',#7282,1.90031);
#2777=CIRCLE('',#7284,1.95469);
#2778=CIRCLE('',#7286,1.90031);
#2779=CIRCLE('',#7289,1.95469);
#2780=CIRCLE('',#7290,1.90031);
#2781=CIRCLE('',#7292,1.95469);
#2782=CIRCLE('',#7294,1.90031);
#2783=CIRCLE('',#7303,0.45);
#2784=CIRCLE('',#7305,0.5);
#2785=CIRCLE('',#7307,0.5);
#2786=CIRCLE('',#7309,0.47);
#2787=CIRCLE('',#7311,0.32);
#2788=CIRCLE('',#7313,0.2942);
#2789=CIRCLE('',#7315,0.2942);
#2790=CIRCLE('',#7317,0.24);
#2791=CIRCLE('',#7329,0.3);
#2792=CIRCLE('',#7331,0.35);
#2793=CIRCLE('',#7333,0.35);
#2794=CIRCLE('',#7335,0.32);
#2795=CIRCLE('',#7337,0.22);
#2796=CIRCLE('',#7339,0.1954);
#2797=CIRCLE('',#7341,0.1954);
#2798=CIRCLE('',#7343,0.16);
#2799=CIRCLE('',#7378,1.25);
#2800=CIRCLE('',#7382,1.25);
#2801=CIRCLE('',#7385,1.25);
#2802=CIRCLE('',#7389,1.25);
#2803=CIRCLE('',#7391,1.6);
#2804=CIRCLE('',#7392,1.25);
#2805=CIRCLE('',#7394,1.6);
#2806=CIRCLE('',#7395,1.25);
#2807=CIRCLE('',#7398,1.25);
#2808=CIRCLE('',#7400,1.25);
#2809=CIRCLE('',#7405,1.255);
#2810=CIRCLE('',#7406,1.255);
#2811=CIRCLE('',#7408,1.7);
#2812=CIRCLE('',#7409,1.7);
#2813=CIRCLE('',#7414,0.21);
#2814=CIRCLE('',#7416,0.21);
#2815=CIRCLE('',#7417,0.21);
#2816=CIRCLE('',#7420,1.255);
#2817=CIRCLE('',#7421,1.255);
#2818=CIRCLE('',#7423,1.8);
#2819=CIRCLE('',#7424,1.8);
#2820=CIRCLE('',#7429,0.21);
#2821=CIRCLE('',#7431,0.21);
#2822=CIRCLE('',#7432,0.21);
#2823=CIRCLE('',#7440,2.);
#2824=CIRCLE('',#7441,1.25);
#2825=CIRCLE('',#7448,1.25);
#2826=CIRCLE('',#7450,2.);
#2827=CIRCLE('',#7455,0.21);
#2828=CIRCLE('',#7457,0.21);
#2829=CIRCLE('',#7458,0.21);
#2830=CIRCLE('',#7464,2.5);
#2831=CIRCLE('',#7465,1.25);
#2832=CIRCLE('',#7467,1.25);
#2833=CIRCLE('',#7469,1.5);
#2834=CIRCLE('',#7470,1.5);
#2835=CIRCLE('',#7472,2.);
#2836=CIRCLE('',#7473,2.);
#2837=CIRCLE('',#7475,2.5);
#2838=CIRCLE('',#7478,2.5);
#2839=CIRCLE('',#7481,2.5);
#2840=CIRCLE('',#7485,1.5);
#2841=CIRCLE('',#7486,1.5);
#2842=CIRCLE('',#7488,1.1);
#2843=CIRCLE('',#7490,1.1);
#2844=CIRCLE('',#7492,2.);
#2845=CIRCLE('',#7493,2.);
#2846=CIRCLE('',#7498,1.5);
#2847=CIRCLE('',#7499,1.5);
#2848=CIRCLE('',#7501,1.1);
#2849=CIRCLE('',#7503,1.1);
#2850=CIRCLE('',#7505,2.);
#2851=CIRCLE('',#7506,2.);
#2852=CIRCLE('',#7529,0.22);
#2853=CIRCLE('',#7531,0.24505);
#2854=CIRCLE('',#7533,0.24505);
#2855=CIRCLE('',#7535,0.175);
#2856=CIRCLE('',#7540,0.976185);
#2857=CIRCLE('',#7541,0.976185);
#2858=CIRCLE('',#7542,0.247676);
#2859=CIRCLE('',#7543,0.976185);
#2860=CIRCLE('',#7544,0.976185);
#2861=CIRCLE('',#7546,0.976185);
#2862=CIRCLE('',#7548,0.5);
#2863=CIRCLE('',#7549,0.5);
#2864=CIRCLE('',#7551,0.56);
#2865=CIRCLE('',#7554,0.976185);
#2866=CIRCLE('',#7556,0.56);
#2867=CIRCLE('',#7560,1.023815);
#2868=CIRCLE('',#7561,1.023815);
#2869=CIRCLE('',#7562,0.247676);
#2870=CIRCLE('',#7563,1.023815);
#2871=CIRCLE('',#7564,1.023815);
#2872=CIRCLE('',#7566,1.023815);
#2873=CIRCLE('',#7568,1.44);
#2874=CIRCLE('',#7569,1.023815);
#2875=CIRCLE('',#7571,1.5);
#2876=CIRCLE('',#7573,1.5);
#2877=CIRCLE('',#7575,1.44);
#2878=CIRCLE('',#7580,0.23815);
#2879=CIRCLE('',#7582,0.23815);
#2880=CIRCLE('',#7584,0.23815);
#2881=CIRCLE('',#7586,0.23815);
#2882=CIRCLE('',#7588,0.23815);
#2883=CIRCLE('',#7590,0.23815);
#2884=CIRCLE('',#7592,0.23815);
#2885=CIRCLE('',#7594,0.23815);
#2886=CIRCLE('',#7597,0.243053047864041);
#2887=CIRCLE('',#7598,0.243053047864041);
#2888=CIRCLE('',#7600,1.019052);
#2889=CIRCLE('',#7601,1.019052);
#2890=CIRCLE('',#7602,1.019052);
#2891=CIRCLE('',#7603,1.019052);
#2892=CIRCLE('',#7604,1.019052);
#2893=CIRCLE('',#7605,1.019052);
#2894=CIRCLE('',#7606,1.019052);
#2895=CIRCLE('',#7607,1.019052);
#2896=CIRCLE('',#7608,1.019052);
#2897=CIRCLE('',#7610,0.980948);
#2898=CIRCLE('',#7611,0.243053047864041);
#2899=CIRCLE('',#7613,0.243053047864041);
#2900=CIRCLE('',#7615,0.980948);
#2901=CIRCLE('',#7616,0.243053047864041);
#2902=CIRCLE('',#7618,0.243053047864041);
#2903=CIRCLE('',#7620,0.980948);
#2904=CIRCLE('',#7621,0.243053047864041);
#2905=CIRCLE('',#7623,0.243053047864041);
#2906=CIRCLE('',#7625,0.980948);
#2907=CIRCLE('',#7626,0.243053047864041);
#2908=CIRCLE('',#7628,0.243053047864041);
#2909=CIRCLE('',#7630,0.980948);
#2910=CIRCLE('',#7631,0.243053047864041);
#2911=CIRCLE('',#7633,0.243053047864041);
#2912=CIRCLE('',#7635,0.980948);
#2913=CIRCLE('',#7636,0.243053047864041);
#2914=CIRCLE('',#7638,0.243053047864041);
#2915=CIRCLE('',#7640,0.980948);
#2916=CIRCLE('',#7641,0.980948);
#2917=CIRCLE('',#7642,0.980948);
#2918=CIRCLE('',#7644,0.243053047864041);
#2919=CIRCLE('',#7646,0.243053047864041);
#2920=CIRCLE('',#7651,1.013815);
#2921=CIRCLE('',#7652,0.991185);
#2922=CIRCLE('',#7654,1.013815);
#2923=CIRCLE('',#7656,0.991185);
#2924=CIRCLE('',#7659,1.013815);
#2925=CIRCLE('',#7660,0.991185);
#2926=CIRCLE('',#7662,1.013815);
#2927=CIRCLE('',#7664,0.991185);
#2928=CIRCLE('',#7687,0.329999999999998);
#2929=CIRCLE('',#7688,0.329999999999998);
#2930=CIRCLE('',#7690,0.505000000000003);
#2931=CIRCLE('',#7691,0.505000000000003);
#2932=CIRCLE('',#7693,0.505000000000003);
#2933=CIRCLE('',#7694,0.505000000000003);
#2934=CIRCLE('',#7707,0.164999999999999);
#2935=CIRCLE('',#7708,0.164999999999999);
#2936=CIRCLE('',#7711,0.164999999999999);
#2937=CIRCLE('',#7712,0.164999999999999);
#2938=CIRCLE('',#7715,0.5);
#2939=CIRCLE('',#7716,0.5);
#2940=CIRCLE('',#7721,0.505000000000003);
#2941=CIRCLE('',#7722,0.505000000000003);
#2942=CIRCLE('',#7724,0.700000000000003);
#2943=CIRCLE('',#7725,0.700000000000003);
#2944=CIRCLE('',#7730,0.505000000000003);
#2945=CIRCLE('',#7731,0.505000000000003);
#2946=CIRCLE('',#7733,0.700000000000003);
#2947=CIRCLE('',#7734,0.700000000000003);
#2948=CIRCLE('',#7739,0.505000000000003);
#2949=CIRCLE('',#7740,0.505000000000003);
#2950=CIRCLE('',#7742,0.700000000000003);
#2951=CIRCLE('',#7743,0.700000000000003);
#2952=CIRCLE('',#7748,0.505000000000003);
#2953=CIRCLE('',#7749,0.505000000000003);
#2954=CIRCLE('',#7751,0.700000000000003);
#2955=CIRCLE('',#7752,0.700000000000003);
#2956=CIRCLE('',#7757,0.225000000000001);
#2957=CIRCLE('',#7758,0.225000000000001);
#2958=CIRCLE('',#7760,0.799999999999997);
#2959=CIRCLE('',#7761,0.799999999999997);
#2960=CIRCLE('',#7766,0.225000000000001);
#2961=CIRCLE('',#7767,0.225000000000001);
#2962=CIRCLE('',#7769,0.799999999999997);
#2963=CIRCLE('',#7770,0.799999999999997);
#2964=CIRCLE('',#7783,0.1954);
#2965=CIRCLE('',#7785,0.3);
#2966=CIRCLE('',#7787,0.35);
#2967=CIRCLE('',#7789,0.35);
#2968=CIRCLE('',#7791,0.32);
#2969=CIRCLE('',#7793,0.22);
#2970=CIRCLE('',#7795,0.1954);
#2971=VERTEX_POINT('',#9929);
#2972=VERTEX_POINT('',#9931);
#2973=VERTEX_POINT('',#9935);
#2974=VERTEX_POINT('',#9937);
#2975=VERTEX_POINT('',#9941);
#2976=VERTEX_POINT('',#9943);
#2977=VERTEX_POINT('',#9947);
#2978=VERTEX_POINT('',#9949);
#2979=VERTEX_POINT('',#9953);
#2980=VERTEX_POINT('',#9954);
#2981=VERTEX_POINT('',#9956);
#2982=VERTEX_POINT('',#9958);
#2983=VERTEX_POINT('',#9962);
#2984=VERTEX_POINT('',#9964);
#2985=VERTEX_POINT('',#9968);
#2986=VERTEX_POINT('',#9970);
#2987=VERTEX_POINT('',#9980);
#2988=VERTEX_POINT('',#9982);
#2989=VERTEX_POINT('',#9987);
#2990=VERTEX_POINT('',#9989);
#2991=VERTEX_POINT('',#9994);
#2992=VERTEX_POINT('',#9996);
#2993=VERTEX_POINT('',#10001);
#2994=VERTEX_POINT('',#10003);
#2995=VERTEX_POINT('',#10008);
#2996=VERTEX_POINT('',#10010);
#2997=VERTEX_POINT('',#10015);
#2998=VERTEX_POINT('',#10017);
#2999=VERTEX_POINT('',#10022);
#3000=VERTEX_POINT('',#10024);
#3001=VERTEX_POINT('',#10029);
#3002=VERTEX_POINT('',#10031);
#3003=VERTEX_POINT('',#10036);
#3004=VERTEX_POINT('',#10037);
#3005=VERTEX_POINT('',#10039);
#3006=VERTEX_POINT('',#10041);
#3007=VERTEX_POINT('',#10045);
#3008=VERTEX_POINT('',#10046);
#3009=VERTEX_POINT('',#10048);
#3010=VERTEX_POINT('',#10050);
#3011=VERTEX_POINT('',#10056);
#3012=VERTEX_POINT('',#10059);
#3013=VERTEX_POINT('',#10060);
#3014=VERTEX_POINT('',#10062);
#3015=VERTEX_POINT('',#10064);
#3016=VERTEX_POINT('',#10068);
#3017=VERTEX_POINT('',#10069);
#3018=VERTEX_POINT('',#10071);
#3019=VERTEX_POINT('',#10073);
#3020=VERTEX_POINT('',#10079);
#3021=VERTEX_POINT('',#10082);
#3022=VERTEX_POINT('',#10083);
#3023=VERTEX_POINT('',#10085);
#3024=VERTEX_POINT('',#10087);
#3025=VERTEX_POINT('',#10091);
#3026=VERTEX_POINT('',#10092);
#3027=VERTEX_POINT('',#10094);
#3028=VERTEX_POINT('',#10096);
#3029=VERTEX_POINT('',#10102);
#3030=VERTEX_POINT('',#10105);
#3031=VERTEX_POINT('',#10106);
#3032=VERTEX_POINT('',#10108);
#3033=VERTEX_POINT('',#10110);
#3034=VERTEX_POINT('',#10114);
#3035=VERTEX_POINT('',#10115);
#3036=VERTEX_POINT('',#10117);
#3037=VERTEX_POINT('',#10119);
#3038=VERTEX_POINT('',#10125);
#3039=VERTEX_POINT('',#10128);
#3040=VERTEX_POINT('',#10130);
#3041=VERTEX_POINT('',#10134);
#3042=VERTEX_POINT('',#10136);
#3043=VERTEX_POINT('',#10140);
#3044=VERTEX_POINT('',#10142);
#3045=VERTEX_POINT('',#10146);
#3046=VERTEX_POINT('',#10148);
#3047=VERTEX_POINT('',#10152);
#3048=VERTEX_POINT('',#10154);
#3049=VERTEX_POINT('',#10156);
#3050=VERTEX_POINT('',#10159);
#3051=VERTEX_POINT('',#10163);
#3052=VERTEX_POINT('',#10167);
#3053=VERTEX_POINT('',#10171);
#3054=VERTEX_POINT('',#10174);
#3055=VERTEX_POINT('',#10176);
#3056=VERTEX_POINT('',#10178);
#3057=VERTEX_POINT('',#10182);
#3058=VERTEX_POINT('',#10186);
#3059=VERTEX_POINT('',#10190);
#3060=VERTEX_POINT('',#10194);
#3061=VERTEX_POINT('',#10198);
#3062=VERTEX_POINT('',#10202);
#3063=VERTEX_POINT('',#10206);
#3064=VERTEX_POINT('',#10210);
#3065=VERTEX_POINT('',#10218);
#3066=VERTEX_POINT('',#10222);
#3067=VERTEX_POINT('',#10230);
#3068=VERTEX_POINT('',#10232);
#3069=VERTEX_POINT('',#10236);
#3070=VERTEX_POINT('',#10238);
#3071=VERTEX_POINT('',#10245);
#3072=VERTEX_POINT('',#10247);
#3073=VERTEX_POINT('',#10251);
#3074=VERTEX_POINT('',#10253);
#3075=VERTEX_POINT('',#10260);
#3076=VERTEX_POINT('',#10262);
#3077=VERTEX_POINT('',#10266);
#3078=VERTEX_POINT('',#10268);
#3079=VERTEX_POINT('',#10272);
#3080=VERTEX_POINT('',#10274);
#3081=VERTEX_POINT('',#10278);
#3082=VERTEX_POINT('',#10280);
#3083=VERTEX_POINT('',#10284);
#3084=VERTEX_POINT('',#10286);
#3085=VERTEX_POINT('',#10290);
#3086=VERTEX_POINT('',#10293);
#3087=VERTEX_POINT('',#10297);
#3088=VERTEX_POINT('',#10299);
#3089=VERTEX_POINT('',#10306);
#3090=VERTEX_POINT('',#10308);
#3091=VERTEX_POINT('',#10312);
#3092=VERTEX_POINT('',#10314);
#3093=VERTEX_POINT('',#10318);
#3094=VERTEX_POINT('',#10320);
#3095=VERTEX_POINT('',#10324);
#3096=VERTEX_POINT('',#10326);
#3097=VERTEX_POINT('',#10330);
#3098=VERTEX_POINT('',#10332);
#3099=VERTEX_POINT('',#10336);
#3100=VERTEX_POINT('',#10339);
#3101=VERTEX_POINT('',#10343);
#3102=VERTEX_POINT('',#10345);
#3103=VERTEX_POINT('',#10352);
#3104=VERTEX_POINT('',#10353);
#3105=VERTEX_POINT('',#10355);
#3106=VERTEX_POINT('',#10357);
#3107=VERTEX_POINT('',#10361);
#3108=VERTEX_POINT('',#10363);
#3109=VERTEX_POINT('',#10367);
#3110=VERTEX_POINT('',#10369);
#3111=VERTEX_POINT('',#10379);
#3112=VERTEX_POINT('',#10380);
#3113=VERTEX_POINT('',#10382);
#3114=VERTEX_POINT('',#10384);
#3115=VERTEX_POINT('',#10388);
#3116=VERTEX_POINT('',#10390);
#3117=VERTEX_POINT('',#10394);
#3118=VERTEX_POINT('',#10396);
#3119=VERTEX_POINT('',#10407);
#3120=VERTEX_POINT('',#10408);
#3121=VERTEX_POINT('',#10411);
#3122=VERTEX_POINT('',#10413);
#3123=VERTEX_POINT('',#10417);
#3124=VERTEX_POINT('',#10421);
#3125=VERTEX_POINT('',#10423);
#3126=VERTEX_POINT('',#10427);
#3127=VERTEX_POINT('',#10432);
#3128=VERTEX_POINT('',#10436);
#3129=VERTEX_POINT('',#10442);
#3130=VERTEX_POINT('',#10443);
#3131=VERTEX_POINT('',#10446);
#3132=VERTEX_POINT('',#10448);
#3133=VERTEX_POINT('',#10452);
#3134=VERTEX_POINT('',#10456);
#3135=VERTEX_POINT('',#10458);
#3136=VERTEX_POINT('',#10461);
#3137=VERTEX_POINT('',#10465);
#3138=VERTEX_POINT('',#10469);
#3139=VERTEX_POINT('',#10477);
#3140=VERTEX_POINT('',#10478);
#3141=VERTEX_POINT('',#10481);
#3142=VERTEX_POINT('',#10482);
#3143=VERTEX_POINT('',#10485);
#3144=VERTEX_POINT('',#10486);
#3145=VERTEX_POINT('',#10489);
#3146=VERTEX_POINT('',#10490);
#3147=VERTEX_POINT('',#10493);
#3148=VERTEX_POINT('',#10494);
#3149=VERTEX_POINT('',#10497);
#3150=VERTEX_POINT('',#10498);
#3151=VERTEX_POINT('',#10501);
#3152=VERTEX_POINT('',#10502);
#3153=VERTEX_POINT('',#10505);
#3154=VERTEX_POINT('',#10506);
#3155=VERTEX_POINT('',#10509);
#3156=VERTEX_POINT('',#10510);
#3157=VERTEX_POINT('',#10514);
#3158=VERTEX_POINT('',#10515);
#3159=VERTEX_POINT('',#10538);
#3160=VERTEX_POINT('',#10540);
#3161=VERTEX_POINT('',#10565);
#3162=VERTEX_POINT('',#10567);
#3163=VERTEX_POINT('',#10590);
#3164=VERTEX_POINT('',#10592);
#3165=VERTEX_POINT('',#10615);
#3166=VERTEX_POINT('',#10617);
#3167=VERTEX_POINT('',#10640);
#3168=VERTEX_POINT('',#10642);
#3169=VERTEX_POINT('',#10645);
#3170=VERTEX_POINT('',#10647);
#3171=VERTEX_POINT('',#10670);
#3172=VERTEX_POINT('',#10672);
#3173=VERTEX_POINT('',#10695);
#3174=VERTEX_POINT('',#10697);
#3175=VERTEX_POINT('',#10720);
#3176=VERTEX_POINT('',#10722);
#3177=VERTEX_POINT('',#10745);
#3178=VERTEX_POINT('',#10747);
#3179=VERTEX_POINT('',#10772);
#3180=VERTEX_POINT('',#10776);
#3181=VERTEX_POINT('',#10801);
#3182=VERTEX_POINT('',#10805);
#3183=VERTEX_POINT('',#10830);
#3184=VERTEX_POINT('',#10834);
#3185=VERTEX_POINT('',#10859);
#3186=VERTEX_POINT('',#10861);
#3187=VERTEX_POINT('',#10865);
#3188=VERTEX_POINT('',#10890);
#3189=VERTEX_POINT('',#10894);
#3190=VERTEX_POINT('',#10919);
#3191=VERTEX_POINT('',#10923);
#3192=VERTEX_POINT('',#10948);
#3193=VERTEX_POINT('',#10952);
#3194=VERTEX_POINT('',#10977);
#3195=VERTEX_POINT('',#10980);
#3196=VERTEX_POINT('',#10982);
#3197=VERTEX_POINT('',#11014);
#3198=VERTEX_POINT('',#11016);
#3199=VERTEX_POINT('',#11019);
#3200=VERTEX_POINT('',#11023);
#3201=VERTEX_POINT('',#11028);
#3202=VERTEX_POINT('',#11030);
#3203=VERTEX_POINT('',#11033);
#3204=VERTEX_POINT('',#11037);
#3205=VERTEX_POINT('',#11048);
#3206=VERTEX_POINT('',#11051);
#3207=VERTEX_POINT('',#11055);
#3208=VERTEX_POINT('',#11059);
#3209=VERTEX_POINT('',#11063);
#3210=VERTEX_POINT('',#11066);
#3211=VERTEX_POINT('',#11070);
#3212=VERTEX_POINT('',#11074);
#3213=VERTEX_POINT('',#11079);
#3214=VERTEX_POINT('',#11080);
#3215=VERTEX_POINT('',#11082);
#3216=VERTEX_POINT('',#11084);
#3217=VERTEX_POINT('',#11088);
#3218=VERTEX_POINT('',#11090);
#3219=VERTEX_POINT('',#11094);
#3220=VERTEX_POINT('',#11096);
#3221=VERTEX_POINT('',#11100);
#3222=VERTEX_POINT('',#11102);
#3223=VERTEX_POINT('',#11106);
#3224=VERTEX_POINT('',#11108);
#3225=VERTEX_POINT('',#11118);
#3226=VERTEX_POINT('',#11121);
#3227=VERTEX_POINT('',#11125);
#3228=VERTEX_POINT('',#11129);
#3229=VERTEX_POINT('',#11133);
#3230=VERTEX_POINT('',#11136);
#3231=VERTEX_POINT('',#11140);
#3232=VERTEX_POINT('',#11144);
#3233=VERTEX_POINT('',#11149);
#3234=VERTEX_POINT('',#11150);
#3235=VERTEX_POINT('',#11152);
#3236=VERTEX_POINT('',#11154);
#3237=VERTEX_POINT('',#11158);
#3238=VERTEX_POINT('',#11160);
#3239=VERTEX_POINT('',#11164);
#3240=VERTEX_POINT('',#11166);
#3241=VERTEX_POINT('',#11170);
#3242=VERTEX_POINT('',#11172);
#3243=VERTEX_POINT('',#11176);
#3244=VERTEX_POINT('',#11178);
#3245=VERTEX_POINT('',#11210);
#3246=VERTEX_POINT('',#11211);
#3247=VERTEX_POINT('',#11213);
#3248=VERTEX_POINT('',#11215);
#3249=VERTEX_POINT('',#11219);
#3250=VERTEX_POINT('',#11221);
#3251=VERTEX_POINT('',#11225);
#3252=VERTEX_POINT('',#11227);
#3253=VERTEX_POINT('',#11235);
#3254=VERTEX_POINT('',#11236);
#3255=VERTEX_POINT('',#11238);
#3256=VERTEX_POINT('',#11240);
#3257=VERTEX_POINT('',#11244);
#3258=VERTEX_POINT('',#11246);
#3259=VERTEX_POINT('',#11250);
#3260=VERTEX_POINT('',#11252);
#3261=VERTEX_POINT('',#11260);
#3262=VERTEX_POINT('',#11262);
#3263=VERTEX_POINT('',#11265);
#3264=VERTEX_POINT('',#11267);
#3265=VERTEX_POINT('',#11272);
#3266=VERTEX_POINT('',#11276);
#3267=VERTEX_POINT('',#11283);
#3268=VERTEX_POINT('',#11285);
#3269=VERTEX_POINT('',#11289);
#3270=VERTEX_POINT('',#11291);
#3271=VERTEX_POINT('',#11298);
#3272=VERTEX_POINT('',#11299);
#3273=VERTEX_POINT('',#11303);
#3274=VERTEX_POINT('',#11318);
#3275=VERTEX_POINT('',#11320);
#3276=VERTEX_POINT('',#11322);
#3277=VERTEX_POINT('',#11359);
#3278=VERTEX_POINT('',#11378);
#3279=VERTEX_POINT('',#11380);
#3280=VERTEX_POINT('',#11384);
#3281=VERTEX_POINT('',#11386);
#3282=VERTEX_POINT('',#11393);
#3283=VERTEX_POINT('',#11394);
#3284=VERTEX_POINT('',#11398);
#3285=VERTEX_POINT('',#11413);
#3286=VERTEX_POINT('',#11415);
#3287=VERTEX_POINT('',#11417);
#3288=VERTEX_POINT('',#11454);
#3289=VERTEX_POINT('',#11473);
#3290=VERTEX_POINT('',#11474);
#3291=VERTEX_POINT('',#11476);
#3292=VERTEX_POINT('',#11478);
#3293=VERTEX_POINT('',#11482);
#3294=VERTEX_POINT('',#11484);
#3295=VERTEX_POINT('',#11486);
#3296=VERTEX_POINT('',#11488);
#3297=VERTEX_POINT('',#11492);
#3298=VERTEX_POINT('',#11494);
#3299=VERTEX_POINT('',#11496);
#3300=VERTEX_POINT('',#11498);
#3301=VERTEX_POINT('',#11506);
#3302=VERTEX_POINT('',#11510);
#3303=VERTEX_POINT('',#11511);
#3304=VERTEX_POINT('',#11513);
#3305=VERTEX_POINT('',#11515);
#3306=VERTEX_POINT('',#11519);
#3307=VERTEX_POINT('',#11521);
#3308=VERTEX_POINT('',#11525);
#3309=VERTEX_POINT('',#11527);
#3310=VERTEX_POINT('',#11537);
#3311=VERTEX_POINT('',#11544);
#3312=VERTEX_POINT('',#11545);
#3313=VERTEX_POINT('',#11549);
#3314=VERTEX_POINT('',#11564);
#3315=VERTEX_POINT('',#11566);
#3316=VERTEX_POINT('',#11568);
#3317=VERTEX_POINT('',#11605);
#3318=VERTEX_POINT('',#11624);
#3319=VERTEX_POINT('',#11625);
#3320=VERTEX_POINT('',#11627);
#3321=VERTEX_POINT('',#11629);
#3322=VERTEX_POINT('',#11633);
#3323=VERTEX_POINT('',#11635);
#3324=VERTEX_POINT('',#11639);
#3325=VERTEX_POINT('',#11641);
#3326=VERTEX_POINT('',#11645);
#3327=VERTEX_POINT('',#11651);
#3328=VERTEX_POINT('',#11653);
#3329=VERTEX_POINT('',#11657);
#3330=VERTEX_POINT('',#11658);
#3331=VERTEX_POINT('',#11660);
#3332=VERTEX_POINT('',#11662);
#3333=VERTEX_POINT('',#11666);
#3334=VERTEX_POINT('',#11668);
#3335=VERTEX_POINT('',#11672);
#3336=VERTEX_POINT('',#11676);
#3337=VERTEX_POINT('',#11682);
#3338=VERTEX_POINT('',#11688);
#3339=VERTEX_POINT('',#11690);
#3340=VERTEX_POINT('',#11694);
#3341=VERTEX_POINT('',#11697);
#3342=VERTEX_POINT('',#11701);
#3343=VERTEX_POINT('',#11703);
#3344=VERTEX_POINT('',#11710);
#3345=VERTEX_POINT('',#11712);
#3346=VERTEX_POINT('',#11716);
#3347=VERTEX_POINT('',#11719);
#3348=VERTEX_POINT('',#11723);
#3349=VERTEX_POINT('',#11725);
#3350=VERTEX_POINT('',#11732);
#3351=VERTEX_POINT('',#11733);
#3352=VERTEX_POINT('',#11735);
#3353=VERTEX_POINT('',#11737);
#3354=VERTEX_POINT('',#11739);
#3355=VERTEX_POINT('',#11741);
#3356=VERTEX_POINT('',#11743);
#3357=VERTEX_POINT('',#11745);
#3358=VERTEX_POINT('',#11749);
#3359=VERTEX_POINT('',#11751);
#3360=VERTEX_POINT('',#11755);
#3361=VERTEX_POINT('',#11759);
#3362=VERTEX_POINT('',#11763);
#3363=VERTEX_POINT('',#11767);
#3364=VERTEX_POINT('',#11769);
#3365=VERTEX_POINT('',#11771);
#3366=VERTEX_POINT('',#11783);
#3367=VERTEX_POINT('',#11784);
#3368=VERTEX_POINT('',#11786);
#3369=VERTEX_POINT('',#11788);
#3370=VERTEX_POINT('',#11792);
#3371=VERTEX_POINT('',#11794);
#3372=VERTEX_POINT('',#11798);
#3373=VERTEX_POINT('',#11800);
#3374=VERTEX_POINT('',#11804);
#3375=VERTEX_POINT('',#11806);
#3376=VERTEX_POINT('',#11810);
#3377=VERTEX_POINT('',#11812);
#3378=VERTEX_POINT('',#11820);
#3379=VERTEX_POINT('',#11823);
#3380=VERTEX_POINT('',#11827);
#3381=VERTEX_POINT('',#11831);
#3382=VERTEX_POINT('',#11838);
#3383=VERTEX_POINT('',#11839);
#3384=VERTEX_POINT('',#11842);
#3385=VERTEX_POINT('',#11844);
#3386=VERTEX_POINT('',#11848);
#3387=VERTEX_POINT('',#11852);
#3388=VERTEX_POINT('',#11854);
#3389=VERTEX_POINT('',#11858);
#3390=VERTEX_POINT('',#11863);
#3391=VERTEX_POINT('',#11867);
#3392=VERTEX_POINT('',#11873);
#3393=VERTEX_POINT('',#11874);
#3394=VERTEX_POINT('',#11877);
#3395=VERTEX_POINT('',#11879);
#3396=VERTEX_POINT('',#11883);
#3397=VERTEX_POINT('',#11887);
#3398=VERTEX_POINT('',#11889);
#3399=VERTEX_POINT('',#11892);
#3400=VERTEX_POINT('',#11896);
#3401=VERTEX_POINT('',#11900);
#3402=VERTEX_POINT('',#11908);
#3403=VERTEX_POINT('',#11909);
#3404=VERTEX_POINT('',#11912);
#3405=VERTEX_POINT('',#11913);
#3406=VERTEX_POINT('',#11916);
#3407=VERTEX_POINT('',#11917);
#3408=VERTEX_POINT('',#11920);
#3409=VERTEX_POINT('',#11921);
#3410=VERTEX_POINT('',#11924);
#3411=VERTEX_POINT('',#11925);
#3412=VERTEX_POINT('',#11928);
#3413=VERTEX_POINT('',#11929);
#3414=VERTEX_POINT('',#11932);
#3415=VERTEX_POINT('',#11933);
#3416=VERTEX_POINT('',#11936);
#3417=VERTEX_POINT('',#11937);
#3418=VERTEX_POINT('',#11941);
#3419=VERTEX_POINT('',#11942);
#3420=VERTEX_POINT('',#11965);
#3421=VERTEX_POINT('',#11967);
#3422=VERTEX_POINT('',#11992);
#3423=VERTEX_POINT('',#11994);
#3424=VERTEX_POINT('',#12017);
#3425=VERTEX_POINT('',#12019);
#3426=VERTEX_POINT('',#12042);
#3427=VERTEX_POINT('',#12044);
#3428=VERTEX_POINT('',#12057);
#3429=VERTEX_POINT('',#12060);
#3430=VERTEX_POINT('',#12073);
#3431=VERTEX_POINT('',#12075);
#3432=VERTEX_POINT('',#12098);
#3433=VERTEX_POINT('',#12100);
#3434=VERTEX_POINT('',#12123);
#3435=VERTEX_POINT('',#12125);
#3436=VERTEX_POINT('',#12148);
#3437=VERTEX_POINT('',#12150);
#3438=VERTEX_POINT('',#12175);
#3439=VERTEX_POINT('',#12179);
#3440=VERTEX_POINT('',#12204);
#3441=VERTEX_POINT('',#12208);
#3442=VERTEX_POINT('',#12233);
#3443=VERTEX_POINT('',#12237);
#3444=VERTEX_POINT('',#12238);
#3445=VERTEX_POINT('',#12265);
#3446=VERTEX_POINT('',#12269);
#3447=VERTEX_POINT('',#12294);
#3448=VERTEX_POINT('',#12298);
#3449=VERTEX_POINT('',#12323);
#3450=VERTEX_POINT('',#12327);
#3451=VERTEX_POINT('',#12352);
#3452=VERTEX_POINT('',#12355);
#3453=VERTEX_POINT('',#12357);
#3454=VERTEX_POINT('',#12389);
#3455=VERTEX_POINT('',#12391);
#3456=VERTEX_POINT('',#12394);
#3457=VERTEX_POINT('',#12398);
#3458=VERTEX_POINT('',#12403);
#3459=VERTEX_POINT('',#12405);
#3460=VERTEX_POINT('',#12408);
#3461=VERTEX_POINT('',#12412);
#3462=VERTEX_POINT('',#12437);
#3463=VERTEX_POINT('',#12439);
#3464=VERTEX_POINT('',#12443);
#3465=VERTEX_POINT('',#12445);
#3466=VERTEX_POINT('',#12449);
#3467=VERTEX_POINT('',#12451);
#3468=VERTEX_POINT('',#12455);
#3469=VERTEX_POINT('',#12456);
#3470=VERTEX_POINT('',#12458);
#3471=VERTEX_POINT('',#12460);
#3472=VERTEX_POINT('',#12464);
#3473=VERTEX_POINT('',#12465);
#3474=VERTEX_POINT('',#12467);
#3475=VERTEX_POINT('',#12469);
#3476=VERTEX_POINT('',#12473);
#3477=VERTEX_POINT('',#12475);
#3478=VERTEX_POINT('',#12482);
#3479=VERTEX_POINT('',#12484);
#3480=VERTEX_POINT('',#12488);
#3481=VERTEX_POINT('',#12489);
#3482=VERTEX_POINT('',#12494);
#3483=VERTEX_POINT('',#12498);
#3484=VERTEX_POINT('',#12506);
#3485=VERTEX_POINT('',#12508);
#3486=VERTEX_POINT('',#12513);
#3487=VERTEX_POINT('',#12515);
#3488=VERTEX_POINT('',#12520);
#3489=VERTEX_POINT('',#12522);
#3490=VERTEX_POINT('',#12529);
#3491=VERTEX_POINT('',#12531);
#3492=VERTEX_POINT('',#12535);
#3493=VERTEX_POINT('',#12537);
#3494=VERTEX_POINT('',#12544);
#3495=VERTEX_POINT('',#12546);
#3496=VERTEX_POINT('',#12550);
#3497=VERTEX_POINT('',#12552);
#3498=VERTEX_POINT('',#12559);
#3499=VERTEX_POINT('',#12561);
#3500=VERTEX_POINT('',#12565);
#3501=VERTEX_POINT('',#12567);
#3502=VERTEX_POINT('',#12574);
#3503=VERTEX_POINT('',#12576);
#3504=VERTEX_POINT('',#12580);
#3505=VERTEX_POINT('',#12582);
#3506=VERTEX_POINT('',#12589);
#3507=VERTEX_POINT('',#12591);
#3508=VERTEX_POINT('',#12595);
#3509=VERTEX_POINT('',#12597);
#3510=VERTEX_POINT('',#12604);
#3511=VERTEX_POINT('',#12606);
#3512=VERTEX_POINT('',#12610);
#3513=VERTEX_POINT('',#12612);
#3514=VERTEX_POINT('',#12619);
#3515=VERTEX_POINT('',#12620);
#3516=VERTEX_POINT('',#12622);
#3517=VERTEX_POINT('',#12624);
#3518=VERTEX_POINT('',#12628);
#3519=VERTEX_POINT('',#12630);
#3520=VERTEX_POINT('',#12634);
#3521=VERTEX_POINT('',#12636);
#3522=VERTEX_POINT('',#12640);
#3523=VERTEX_POINT('',#12642);
#3524=VERTEX_POINT('',#12646);
#3525=VERTEX_POINT('',#12648);
#3526=VERTEX_POINT('',#12657);
#3527=VERTEX_POINT('',#12660);
#3528=VERTEX_POINT('',#12663);
#3529=VERTEX_POINT('',#12667);
#3530=VERTEX_POINT('',#12671);
#3531=VERTEX_POINT('',#12675);
#3532=VERTEX_POINT('',#12678);
#3533=EDGE_CURVE('',#2971,#2971,#2616,.T.);
#3534=EDGE_CURVE('',#2971,#2972,#1786,.T.);
#3535=EDGE_CURVE('',#2972,#2972,#2617,.T.);
#3536=EDGE_CURVE('',#2973,#2973,#2618,.T.);
#3537=EDGE_CURVE('',#2973,#2974,#1787,.T.);
#3538=EDGE_CURVE('',#2974,#2974,#2619,.T.);
#3539=EDGE_CURVE('',#2975,#2975,#2620,.T.);
#3540=EDGE_CURVE('',#2975,#2976,#1788,.T.);
#3541=EDGE_CURVE('',#2976,#2976,#2621,.T.);
#3542=EDGE_CURVE('',#2977,#2977,#2622,.T.);
#3543=EDGE_CURVE('',#2977,#2978,#1789,.T.);
#3544=EDGE_CURVE('',#2978,#2978,#2623,.T.);
#3545=EDGE_CURVE('',#2979,#2980,#1790,.T.);
#3546=EDGE_CURVE('',#2980,#2981,#1791,.T.);
#3547=EDGE_CURVE('',#2982,#2981,#1792,.T.);
#3548=EDGE_CURVE('',#2979,#2982,#1793,.T.);
#3549=EDGE_CURVE('',#2983,#2979,#1794,.T.);
#3550=EDGE_CURVE('',#2984,#2982,#1795,.T.);
#3551=EDGE_CURVE('',#2983,#2984,#1796,.T.);
#3552=EDGE_CURVE('',#2985,#2983,#1797,.T.);
#3553=EDGE_CURVE('',#2986,#2984,#1798,.T.);
#3554=EDGE_CURVE('',#2985,#2986,#1799,.T.);
#3555=EDGE_CURVE('',#2980,#2985,#1800,.T.);
#3556=EDGE_CURVE('',#2981,#2986,#1801,.T.);
#3557=EDGE_CURVE('',#2987,#2987,#2624,.T.);
#3558=EDGE_CURVE('',#2987,#2988,#1802,.T.);
#3559=EDGE_CURVE('',#2988,#2988,#2625,.T.);
#3560=EDGE_CURVE('',#2989,#2989,#2626,.T.);
#3561=EDGE_CURVE('',#2989,#2990,#1803,.T.);
#3562=EDGE_CURVE('',#2990,#2990,#2627,.T.);
#3563=EDGE_CURVE('',#2991,#2991,#2628,.T.);
#3564=EDGE_CURVE('',#2991,#2992,#1804,.T.);
#3565=EDGE_CURVE('',#2992,#2992,#2629,.T.);
#3566=EDGE_CURVE('',#2993,#2993,#2630,.T.);
#3567=EDGE_CURVE('',#2993,#2994,#1805,.T.);
#3568=EDGE_CURVE('',#2994,#2994,#2631,.T.);
#3569=EDGE_CURVE('',#2995,#2995,#2632,.T.);
#3570=EDGE_CURVE('',#2995,#2996,#1806,.T.);
#3571=EDGE_CURVE('',#2996,#2996,#2633,.T.);
#3572=EDGE_CURVE('',#2997,#2997,#2634,.T.);
#3573=EDGE_CURVE('',#2997,#2998,#1807,.T.);
#3574=EDGE_CURVE('',#2998,#2998,#2635,.T.);
#3575=EDGE_CURVE('',#2999,#2999,#2636,.T.);
#3576=EDGE_CURVE('',#2999,#3000,#1808,.T.);
#3577=EDGE_CURVE('',#3000,#3000,#2637,.T.);
#3578=EDGE_CURVE('',#3001,#3001,#2638,.T.);
#3579=EDGE_CURVE('',#3001,#3002,#1809,.T.);
#3580=EDGE_CURVE('',#3002,#3002,#2639,.T.);
#3581=EDGE_CURVE('',#3003,#3004,#1810,.T.);
#3582=EDGE_CURVE('',#3005,#3003,#2640,.T.);
#3583=EDGE_CURVE('',#3006,#3005,#1811,.T.);
#3584=EDGE_CURVE('',#3004,#3006,#2641,.T.);
#3585=EDGE_CURVE('',#3007,#3008,#1812,.T.);
#3586=EDGE_CURVE('',#3009,#3007,#2642,.T.);
#3587=EDGE_CURVE('',#3010,#3009,#1813,.T.);
#3588=EDGE_CURVE('',#3008,#3010,#2643,.T.);
#3589=EDGE_CURVE('',#3004,#3007,#1814,.T.);
#3590=EDGE_CURVE('',#3009,#3006,#1815,.T.);
#3591=EDGE_CURVE('',#3011,#3011,#2644,.T.);
#3592=EDGE_CURVE('',#3012,#3013,#1816,.T.);
#3593=EDGE_CURVE('',#3014,#3012,#2645,.T.);
#3594=EDGE_CURVE('',#3015,#3014,#1817,.T.);
#3595=EDGE_CURVE('',#3013,#3015,#2646,.T.);
#3596=EDGE_CURVE('',#3016,#3017,#1818,.T.);
#3597=EDGE_CURVE('',#3018,#3016,#2647,.T.);
#3598=EDGE_CURVE('',#3019,#3018,#1819,.T.);
#3599=EDGE_CURVE('',#3017,#3019,#2648,.T.);
#3600=EDGE_CURVE('',#3013,#3016,#1820,.T.);
#3601=EDGE_CURVE('',#3018,#3015,#1821,.T.);
#3602=EDGE_CURVE('',#3020,#3020,#2649,.T.);
#3603=EDGE_CURVE('',#3021,#3022,#1822,.T.);
#3604=EDGE_CURVE('',#3023,#3021,#2650,.T.);
#3605=EDGE_CURVE('',#3024,#3023,#1823,.T.);
#3606=EDGE_CURVE('',#3022,#3024,#2651,.T.);
#3607=EDGE_CURVE('',#3025,#3026,#1824,.T.);
#3608=EDGE_CURVE('',#3027,#3025,#2652,.T.);
#3609=EDGE_CURVE('',#3028,#3027,#1825,.T.);
#3610=EDGE_CURVE('',#3026,#3028,#2653,.T.);
#3611=EDGE_CURVE('',#3022,#3025,#1826,.T.);
#3612=EDGE_CURVE('',#3027,#3024,#1827,.T.);
#3613=EDGE_CURVE('',#3029,#3029,#2654,.T.);
#3614=EDGE_CURVE('',#3030,#3031,#1828,.T.);
#3615=EDGE_CURVE('',#3032,#3030,#2655,.T.);
#3616=EDGE_CURVE('',#3033,#3032,#1829,.T.);
#3617=EDGE_CURVE('',#3031,#3033,#2656,.T.);
#3618=EDGE_CURVE('',#3034,#3035,#1830,.T.);
#3619=EDGE_CURVE('',#3036,#3034,#2657,.T.);
#3620=EDGE_CURVE('',#3037,#3036,#1831,.T.);
#3621=EDGE_CURVE('',#3035,#3037,#2658,.T.);
#3622=EDGE_CURVE('',#3031,#3034,#1832,.T.);
#3623=EDGE_CURVE('',#3036,#3033,#1833,.T.);
#3624=EDGE_CURVE('',#3038,#3038,#2659,.T.);
#3625=EDGE_CURVE('',#3039,#3003,#1834,.T.);
#3626=EDGE_CURVE('',#3039,#3040,#1835,.T.);
#3627=EDGE_CURVE('',#3005,#3040,#1836,.T.);
#3628=EDGE_CURVE('',#3041,#3010,#1837,.T.);
#3629=EDGE_CURVE('',#3042,#3041,#1838,.T.);
#3630=EDGE_CURVE('',#3008,#3042,#1839,.T.);
#3631=EDGE_CURVE('',#3043,#3012,#1840,.T.);
#3632=EDGE_CURVE('',#3044,#3043,#1841,.T.);
#3633=EDGE_CURVE('',#3014,#3044,#1842,.T.);
#3634=EDGE_CURVE('',#3045,#3019,#1843,.T.);
#3635=EDGE_CURVE('',#3046,#3045,#1844,.T.);
#3636=EDGE_CURVE('',#3017,#3046,#1845,.T.);
#3637=EDGE_CURVE('',#3040,#3047,#1846,.T.);
#3638=EDGE_CURVE('',#3047,#3048,#1847,.T.);
#3639=EDGE_CURVE('',#3048,#3049,#1848,.T.);
#3640=EDGE_CURVE('',#3049,#3028,#1849,.T.);
#3641=EDGE_CURVE('',#3023,#3050,#1850,.T.);
#3642=EDGE_CURVE('',#3041,#3050,#2660,.T.);
#3643=EDGE_CURVE('',#3051,#3021,#1851,.T.);
#3644=EDGE_CURVE('',#3050,#3051,#1852,.T.);
#3645=EDGE_CURVE('',#3052,#3049,#1853,.T.);
#3646=EDGE_CURVE('',#3026,#3052,#1854,.T.);
#3647=EDGE_CURVE('',#3053,#3044,#2661,.T.);
#3648=EDGE_CURVE('',#3053,#3037,#1855,.T.);
#3649=EDGE_CURVE('',#3032,#3054,#1856,.T.);
#3650=EDGE_CURVE('',#3054,#3055,#1857,.T.);
#3651=EDGE_CURVE('',#3055,#3056,#1858,.T.);
#3652=EDGE_CURVE('',#3056,#3045,#1859,.T.);
#3653=EDGE_CURVE('',#3057,#3030,#1860,.T.);
#3654=EDGE_CURVE('',#3057,#3054,#1861,.T.);
#3655=EDGE_CURVE('',#3058,#3053,#1862,.T.);
#3656=EDGE_CURVE('',#3035,#3058,#1863,.T.);
#3657=EDGE_CURVE('',#3059,#3059,#2662,.T.);
#3658=EDGE_CURVE('',#3059,#3011,#1864,.T.);
#3659=EDGE_CURVE('',#3060,#3060,#2663,.T.);
#3660=EDGE_CURVE('',#3060,#3020,#1865,.T.);
#3661=EDGE_CURVE('',#3061,#3061,#2664,.T.);
#3662=EDGE_CURVE('',#3061,#3029,#1866,.T.);
#3663=EDGE_CURVE('',#3062,#3062,#2665,.T.);
#3664=EDGE_CURVE('',#3062,#3038,#1867,.T.);
#3665=EDGE_CURVE('',#3046,#3063,#1868,.T.);
#3666=EDGE_CURVE('',#3063,#3056,#1869,.T.);
#3667=EDGE_CURVE('',#3063,#3064,#1870,.T.);
#3668=EDGE_CURVE('',#3064,#3055,#1871,.T.);
#3669=EDGE_CURVE('',#3064,#3057,#1872,.T.);
#3670=EDGE_CURVE('',#3043,#3058,#2666,.T.);
#3671=EDGE_CURVE('',#3052,#3065,#1873,.T.);
#3672=EDGE_CURVE('',#3065,#3048,#1874,.T.);
#3673=EDGE_CURVE('',#3065,#3066,#1875,.T.);
#3674=EDGE_CURVE('',#3066,#3047,#1876,.T.);
#3675=EDGE_CURVE('',#3066,#3039,#1877,.T.);
#3676=EDGE_CURVE('',#3051,#3042,#2667,.T.);
#3677=EDGE_CURVE('',#3067,#3067,#2668,.T.);
#3678=EDGE_CURVE('',#3067,#3068,#1878,.T.);
#3679=EDGE_CURVE('',#3068,#3068,#2669,.T.);
#3680=EDGE_CURVE('',#3069,#3069,#2670,.T.);
#3681=EDGE_CURVE('',#3069,#3070,#1879,.T.);
#3682=EDGE_CURVE('',#3070,#3070,#2671,.T.);
#3683=EDGE_CURVE('',#3071,#3071,#2672,.T.);
#3684=EDGE_CURVE('',#3071,#3072,#1880,.T.);
#3685=EDGE_CURVE('',#3072,#3072,#2673,.T.);
#3686=EDGE_CURVE('',#3073,#3073,#2674,.T.);
#3687=EDGE_CURVE('',#3073,#3074,#1881,.T.);
#3688=EDGE_CURVE('',#3074,#3074,#2675,.T.);
#3689=EDGE_CURVE('',#3075,#3075,#2676,.T.);
#3690=EDGE_CURVE('',#3075,#3076,#1882,.T.);
#3691=EDGE_CURVE('',#3076,#3076,#2677,.T.);
#3692=EDGE_CURVE('',#3077,#3077,#2678,.T.);
#3693=EDGE_CURVE('',#3077,#3078,#1883,.T.);
#3694=EDGE_CURVE('',#3078,#3078,#2679,.T.);
#3695=EDGE_CURVE('',#3079,#3079,#2680,.T.);
#3696=EDGE_CURVE('',#3079,#3080,#1884,.T.);
#3697=EDGE_CURVE('',#3080,#3080,#2681,.T.);
#3698=EDGE_CURVE('',#3081,#3081,#2682,.T.);
#3699=EDGE_CURVE('',#3081,#3082,#1885,.T.);
#3700=EDGE_CURVE('',#3082,#3082,#2683,.T.);
#3701=EDGE_CURVE('',#3083,#3083,#2684,.T.);
#3702=EDGE_CURVE('',#3083,#3084,#1886,.T.);
#3703=EDGE_CURVE('',#3084,#3084,#2685,.T.);
#3704=EDGE_CURVE('',#3085,#3085,#2686,.T.);
#3705=EDGE_CURVE('',#3085,#3086,#1887,.T.);
#3706=EDGE_CURVE('',#3086,#3086,#2687,.T.);
#3707=EDGE_CURVE('',#3087,#3087,#2688,.T.);
#3708=EDGE_CURVE('',#3087,#3088,#1888,.T.);
#3709=EDGE_CURVE('',#3088,#3088,#2689,.T.);
#3710=EDGE_CURVE('',#3089,#3089,#2690,.T.);
#3711=EDGE_CURVE('',#3089,#3090,#1889,.T.);
#3712=EDGE_CURVE('',#3090,#3090,#2691,.T.);
#3713=EDGE_CURVE('',#3091,#3091,#2692,.T.);
#3714=EDGE_CURVE('',#3091,#3092,#1890,.T.);
#3715=EDGE_CURVE('',#3092,#3092,#2693,.T.);
#3716=EDGE_CURVE('',#3093,#3093,#2694,.T.);
#3717=EDGE_CURVE('',#3093,#3094,#1891,.T.);
#3718=EDGE_CURVE('',#3094,#3094,#2695,.T.);
#3719=EDGE_CURVE('',#3095,#3095,#2696,.T.);
#3720=EDGE_CURVE('',#3095,#3096,#1892,.T.);
#3721=EDGE_CURVE('',#3096,#3096,#2697,.T.);
#3722=EDGE_CURVE('',#3097,#3097,#2698,.T.);
#3723=EDGE_CURVE('',#3097,#3098,#1893,.T.);
#3724=EDGE_CURVE('',#3098,#3098,#2699,.T.);
#3725=EDGE_CURVE('',#3099,#3099,#2700,.T.);
#3726=EDGE_CURVE('',#3100,#3100,#2701,.T.);
#3727=EDGE_CURVE('',#3100,#3099,#1894,.T.);
#3728=EDGE_CURVE('',#3101,#3101,#2702,.T.);
#3729=EDGE_CURVE('',#3101,#3102,#1895,.T.);
#3730=EDGE_CURVE('',#3102,#3102,#2703,.T.);
#3731=EDGE_CURVE('',#3103,#3104,#1896,.T.);
#3732=EDGE_CURVE('',#3104,#3105,#1897,.T.);
#3733=EDGE_CURVE('',#3106,#3105,#1898,.T.);
#3734=EDGE_CURVE('',#3103,#3106,#1899,.T.);
#3735=EDGE_CURVE('',#3107,#3103,#1900,.T.);
#3736=EDGE_CURVE('',#3108,#3106,#1901,.T.);
#3737=EDGE_CURVE('',#3107,#3108,#1902,.T.);
#3738=EDGE_CURVE('',#3109,#3107,#1903,.T.);
#3739=EDGE_CURVE('',#3110,#3108,#1904,.T.);
#3740=EDGE_CURVE('',#3109,#3110,#1905,.T.);
#3741=EDGE_CURVE('',#3104,#3109,#1906,.T.);
#3742=EDGE_CURVE('',#3105,#3110,#1907,.T.);
#3743=EDGE_CURVE('',#3111,#3112,#1908,.T.);
#3744=EDGE_CURVE('',#3112,#3113,#1909,.T.);
#3745=EDGE_CURVE('',#3114,#3113,#1910,.T.);
#3746=EDGE_CURVE('',#3111,#3114,#1911,.T.);
#3747=EDGE_CURVE('',#3115,#3111,#1912,.T.);
#3748=EDGE_CURVE('',#3116,#3114,#1913,.T.);
#3749=EDGE_CURVE('',#3115,#3116,#1914,.T.);
#3750=EDGE_CURVE('',#3117,#3115,#1915,.T.);
#3751=EDGE_CURVE('',#3118,#3116,#1916,.T.);
#3752=EDGE_CURVE('',#3117,#3118,#1917,.T.);
#3753=EDGE_CURVE('',#3112,#3117,#1918,.T.);
#3754=EDGE_CURVE('',#3113,#3118,#1919,.T.);
#3755=EDGE_CURVE('',#3119,#3120,#2704,.T.);
#3756=EDGE_CURVE('',#3120,#3119,#2705,.T.);
#3757=EDGE_CURVE('',#3120,#3121,#2706,.T.);
#3758=EDGE_CURVE('',#3122,#3121,#2707,.T.);
#3759=EDGE_CURVE('',#3121,#3122,#2708,.T.);
#3760=EDGE_CURVE('',#3122,#3123,#1920,.T.);
#3761=EDGE_CURVE('',#3123,#3123,#2709,.T.);
#3762=EDGE_CURVE('',#3124,#3124,#2710,.T.);
#3763=EDGE_CURVE('',#3124,#3125,#1921,.T.);
#3764=EDGE_CURVE('',#3125,#3125,#2711,.T.);
#3765=EDGE_CURVE('',#3125,#3126,#1922,.T.);
#3766=EDGE_CURVE('',#3126,#3126,#2712,.T.);
#3767=EDGE_CURVE('',#3127,#3127,#2713,.T.);
#3768=EDGE_CURVE('',#3127,#3119,#1923,.T.);
#3769=EDGE_CURVE('',#3128,#3128,#2714,.T.);
#3770=EDGE_CURVE('',#3128,#3124,#1924,.T.);
#3771=EDGE_CURVE('',#3129,#3130,#2715,.T.);
#3772=EDGE_CURVE('',#3130,#3129,#2716,.T.);
#3773=EDGE_CURVE('',#3130,#3131,#2717,.T.);
#3774=EDGE_CURVE('',#3132,#3131,#2718,.T.);
#3775=EDGE_CURVE('',#3131,#3132,#2719,.T.);
#3776=EDGE_CURVE('',#3133,#3133,#2720,.T.);
#3777=EDGE_CURVE('',#3133,#3132,#1925,.T.);
#3778=EDGE_CURVE('',#3134,#3134,#2721,.T.);
#3779=EDGE_CURVE('',#3135,#3135,#2722,.T.);
#3780=EDGE_CURVE('',#3136,#3136,#2723,.T.);
#3781=EDGE_CURVE('',#3136,#3134,#1926,.T.);
#3782=EDGE_CURVE('',#3137,#3137,#2724,.T.);
#3783=EDGE_CURVE('',#3137,#3136,#1927,.T.);
#3784=EDGE_CURVE('',#3138,#3138,#2725,.T.);
#3785=EDGE_CURVE('',#3138,#3137,#1928,.T.);
#3786=EDGE_CURVE('',#3129,#3135,#1929,.T.);
#3787=EDGE_CURVE('',#3139,#3140,#2726,.T.);
#3788=EDGE_CURVE('',#3141,#3142,#2727,.T.);
#3789=EDGE_CURVE('',#3143,#3144,#2728,.T.);
#3790=EDGE_CURVE('',#3145,#3146,#2729,.T.);
#3791=EDGE_CURVE('',#3147,#3148,#2730,.T.);
#3792=EDGE_CURVE('',#3149,#3150,#2731,.T.);
#3793=EDGE_CURVE('',#3151,#3152,#2732,.T.);
#3794=EDGE_CURVE('',#3153,#3154,#2733,.T.);
#3795=EDGE_CURVE('',#3155,#3156,#2734,.T.);
#3796=EDGE_CURVE('',#3157,#3158,#245,.T.);
#3797=EDGE_CURVE('',#3159,#3157,#2735,.T.);
#3798=EDGE_CURVE('',#3160,#3159,#246,.T.);
#3799=EDGE_CURVE('',#3158,#3160,#2736,.T.);
#3800=EDGE_CURVE('',#3161,#3159,#2737,.T.);
#3801=EDGE_CURVE('',#3161,#3162,#247,.T.);
#3802=EDGE_CURVE('',#3163,#3162,#2738,.T.);
#3803=EDGE_CURVE('',#3163,#3164,#248,.T.);
#3804=EDGE_CURVE('',#3165,#3164,#2739,.T.);
#3805=EDGE_CURVE('',#3165,#3166,#249,.T.);
#3806=EDGE_CURVE('',#3167,#3166,#2740,.T.);
#3807=EDGE_CURVE('',#3167,#3168,#1930,.T.);
#3808=EDGE_CURVE('',#3168,#3168,#2741,.T.);
#3809=EDGE_CURVE('',#3169,#3167,#2742,.T.);
#3810=EDGE_CURVE('',#3169,#3170,#250,.T.);
#3811=EDGE_CURVE('',#3171,#3170,#2743,.T.);
#3812=EDGE_CURVE('',#3171,#3172,#251,.T.);
#3813=EDGE_CURVE('',#3173,#3172,#2744,.T.);
#3814=EDGE_CURVE('',#3173,#3174,#252,.T.);
#3815=EDGE_CURVE('',#3175,#3174,#2745,.T.);
#3816=EDGE_CURVE('',#3175,#3176,#253,.T.);
#3817=EDGE_CURVE('',#3177,#3176,#2746,.T.);
#3818=EDGE_CURVE('',#3177,#3178,#254,.T.);
#3819=EDGE_CURVE('',#3160,#3178,#2747,.T.);
#3820=EDGE_CURVE('',#3157,#3179,#2748,.T.);
#3821=EDGE_CURVE('',#3179,#3161,#2749,.T.);
#3822=EDGE_CURVE('',#3180,#3179,#255,.T.);
#3823=EDGE_CURVE('',#3162,#3180,#2750,.T.);
#3824=EDGE_CURVE('',#3180,#3181,#2751,.T.);
#3825=EDGE_CURVE('',#3181,#3163,#2752,.T.);
#3826=EDGE_CURVE('',#3182,#3181,#256,.T.);
#3827=EDGE_CURVE('',#3164,#3182,#2753,.T.);
#3828=EDGE_CURVE('',#3182,#3183,#2754,.T.);
#3829=EDGE_CURVE('',#3183,#3165,#2755,.T.);
#3830=EDGE_CURVE('',#3184,#3183,#257,.T.);
#3831=EDGE_CURVE('',#3166,#3184,#2756,.T.);
#3832=EDGE_CURVE('',#3184,#3185,#2757,.T.);
#3833=EDGE_CURVE('',#3185,#3186,#2758,.T.);
#3834=EDGE_CURVE('',#3186,#3169,#2759,.T.);
#3835=EDGE_CURVE('',#3187,#3186,#258,.T.);
#3836=EDGE_CURVE('',#3170,#3187,#2760,.T.);
#3837=EDGE_CURVE('',#3187,#3188,#2761,.T.);
#3838=EDGE_CURVE('',#3188,#3171,#2762,.T.);
#3839=EDGE_CURVE('',#3189,#3188,#259,.T.);
#3840=EDGE_CURVE('',#3172,#3189,#2763,.T.);
#3841=EDGE_CURVE('',#3189,#3190,#2764,.T.);
#3842=EDGE_CURVE('',#3190,#3173,#2765,.T.);
#3843=EDGE_CURVE('',#3191,#3190,#260,.T.);
#3844=EDGE_CURVE('',#3174,#3191,#2766,.T.);
#3845=EDGE_CURVE('',#3191,#3192,#2767,.T.);
#3846=EDGE_CURVE('',#3192,#3175,#2768,.T.);
#3847=EDGE_CURVE('',#3193,#3192,#261,.T.);
#3848=EDGE_CURVE('',#3176,#3193,#2769,.T.);
#3849=EDGE_CURVE('',#3194,#3194,#2770,.T.);
#3850=EDGE_CURVE('',#3194,#3185,#1931,.T.);
#3851=EDGE_CURVE('',#3195,#3158,#2771,.T.);
#3852=EDGE_CURVE('',#3195,#3196,#262,.T.);
#3853=EDGE_CURVE('',#3193,#3196,#2772,.T.);
#3854=EDGE_CURVE('',#3178,#3195,#2773,.T.);
#3855=EDGE_CURVE('',#3196,#3177,#2774,.T.);
#3856=EDGE_CURVE('',#3197,#3197,#2775,.T.);
#3857=EDGE_CURVE('',#3198,#3198,#2776,.T.);
#3858=EDGE_CURVE('',#3199,#3199,#2777,.T.);
#3859=EDGE_CURVE('',#3199,#3197,#1932,.T.);
#3860=EDGE_CURVE('',#3200,#3200,#2778,.T.);
#3861=EDGE_CURVE('',#3200,#3198,#1933,.T.);
#3862=EDGE_CURVE('',#3201,#3201,#2779,.T.);
#3863=EDGE_CURVE('',#3202,#3202,#2780,.T.);
#3864=EDGE_CURVE('',#3203,#3203,#2781,.T.);
#3865=EDGE_CURVE('',#3203,#3201,#1934,.T.);
#3866=EDGE_CURVE('',#3204,#3204,#2782,.T.);
#3867=EDGE_CURVE('',#3204,#3202,#1935,.T.);
#3868=EDGE_CURVE('',#3205,#3205,#2783,.T.);
#3869=EDGE_CURVE('',#3206,#3206,#2784,.T.);
#3870=EDGE_CURVE('',#3206,#3205,#1936,.T.);
#3871=EDGE_CURVE('',#3207,#3207,#2785,.T.);
#3872=EDGE_CURVE('',#3207,#3206,#1937,.T.);
#3873=EDGE_CURVE('',#3208,#3208,#2786,.T.);
#3874=EDGE_CURVE('',#3208,#3207,#1938,.T.);
#3875=EDGE_CURVE('',#3209,#3209,#2787,.T.);
#3876=EDGE_CURVE('',#3210,#3210,#2788,.F.);
#3877=EDGE_CURVE('',#3210,#3209,#1939,.T.);
#3878=EDGE_CURVE('',#3211,#3211,#2789,.F.);
#3879=EDGE_CURVE('',#3211,#3210,#1940,.T.);
#3880=EDGE_CURVE('',#3212,#3212,#2790,.T.);
#3881=EDGE_CURVE('',#3212,#3211,#1941,.T.);
#3882=EDGE_CURVE('',#3213,#3214,#1942,.T.);
#3883=EDGE_CURVE('',#3214,#3215,#1943,.T.);
#3884=EDGE_CURVE('',#3215,#3216,#1944,.T.);
#3885=EDGE_CURVE('',#3213,#3216,#1945,.T.);
#3886=EDGE_CURVE('',#3214,#3217,#1946,.T.);
#3887=EDGE_CURVE('',#3217,#3218,#1947,.T.);
#3888=EDGE_CURVE('',#3218,#3215,#1948,.T.);
#3889=EDGE_CURVE('',#3217,#3219,#1949,.T.);
#3890=EDGE_CURVE('',#3219,#3220,#1950,.T.);
#3891=EDGE_CURVE('',#3220,#3218,#1951,.T.);
#3892=EDGE_CURVE('',#3219,#3221,#1952,.T.);
#3893=EDGE_CURVE('',#3221,#3222,#1953,.T.);
#3894=EDGE_CURVE('',#3222,#3220,#1954,.T.);
#3895=EDGE_CURVE('',#3221,#3223,#1955,.T.);
#3896=EDGE_CURVE('',#3223,#3224,#1956,.T.);
#3897=EDGE_CURVE('',#3224,#3222,#1957,.T.);
#3898=EDGE_CURVE('',#3223,#3213,#1958,.T.);
#3899=EDGE_CURVE('',#3216,#3224,#1959,.T.);
#3900=EDGE_CURVE('',#3225,#3225,#2791,.T.);
#3901=EDGE_CURVE('',#3226,#3226,#2792,.T.);
#3902=EDGE_CURVE('',#3226,#3225,#1960,.T.);
#3903=EDGE_CURVE('',#3227,#3227,#2793,.T.);
#3904=EDGE_CURVE('',#3227,#3226,#1961,.T.);
#3905=EDGE_CURVE('',#3228,#3228,#2794,.T.);
#3906=EDGE_CURVE('',#3228,#3227,#1962,.T.);
#3907=EDGE_CURVE('',#3229,#3229,#2795,.T.);
#3908=EDGE_CURVE('',#3230,#3230,#2796,.F.);
#3909=EDGE_CURVE('',#3230,#3229,#1963,.T.);
#3910=EDGE_CURVE('',#3231,#3231,#2797,.F.);
#3911=EDGE_CURVE('',#3231,#3230,#1964,.T.);
#3912=EDGE_CURVE('',#3232,#3232,#2798,.T.);
#3913=EDGE_CURVE('',#3232,#3231,#1965,.T.);
#3914=EDGE_CURVE('',#3233,#3234,#1966,.T.);
#3915=EDGE_CURVE('',#3234,#3235,#1967,.T.);
#3916=EDGE_CURVE('',#3235,#3236,#1968,.T.);
#3917=EDGE_CURVE('',#3233,#3236,#1969,.T.);
#3918=EDGE_CURVE('',#3234,#3237,#1970,.T.);
#3919=EDGE_CURVE('',#3237,#3238,#1971,.T.);
#3920=EDGE_CURVE('',#3238,#3235,#1972,.T.);
#3921=EDGE_CURVE('',#3237,#3239,#1973,.T.);
#3922=EDGE_CURVE('',#3239,#3240,#1974,.T.);
#3923=EDGE_CURVE('',#3240,#3238,#1975,.T.);
#3924=EDGE_CURVE('',#3239,#3241,#1976,.T.);
#3925=EDGE_CURVE('',#3241,#3242,#1977,.T.);
#3926=EDGE_CURVE('',#3242,#3240,#1978,.T.);
#3927=EDGE_CURVE('',#3241,#3243,#1979,.T.);
#3928=EDGE_CURVE('',#3243,#3244,#1980,.T.);
#3929=EDGE_CURVE('',#3244,#3242,#1981,.T.);
#3930=EDGE_CURVE('',#3243,#3233,#1982,.T.);
#3931=EDGE_CURVE('',#3236,#3244,#1983,.T.);
#3932=EDGE_CURVE('',#3245,#3246,#1984,.T.);
#3933=EDGE_CURVE('',#3245,#3247,#1985,.T.);
#3934=EDGE_CURVE('',#3248,#3247,#1986,.T.);
#3935=EDGE_CURVE('',#3248,#3246,#1987,.T.);
#3936=EDGE_CURVE('',#3246,#3249,#2799,.T.);
#3937=EDGE_CURVE('',#3250,#3248,#1988,.T.);
#3938=EDGE_CURVE('',#3249,#3250,#1989,.T.);
#3939=EDGE_CURVE('',#3249,#3251,#1990,.T.);
#3940=EDGE_CURVE('',#3250,#3252,#1991,.T.);
#3941=EDGE_CURVE('',#3252,#3251,#1992,.T.);
#3942=EDGE_CURVE('',#3247,#3252,#1993,.T.);
#3943=EDGE_CURVE('',#3251,#3245,#2800,.T.);
#3944=EDGE_CURVE('',#3253,#3254,#1994,.T.);
#3945=EDGE_CURVE('',#3253,#3255,#1995,.T.);
#3946=EDGE_CURVE('',#3256,#3255,#1996,.T.);
#3947=EDGE_CURVE('',#3256,#3254,#1997,.T.);
#3948=EDGE_CURVE('',#3254,#3257,#2801,.T.);
#3949=EDGE_CURVE('',#3258,#3256,#1998,.T.);
#3950=EDGE_CURVE('',#3257,#3258,#1999,.T.);
#3951=EDGE_CURVE('',#3257,#3259,#2000,.T.);
#3952=EDGE_CURVE('',#3258,#3260,#2001,.T.);
#3953=EDGE_CURVE('',#3260,#3259,#2002,.T.);
#3954=EDGE_CURVE('',#3255,#3260,#2003,.T.);
#3955=EDGE_CURVE('',#3259,#3253,#2802,.T.);
#3956=EDGE_CURVE('',#3261,#3261,#2803,.T.);
#3957=EDGE_CURVE('',#3262,#3262,#2804,.T.);
#3958=EDGE_CURVE('',#3263,#3263,#2805,.T.);
#3959=EDGE_CURVE('',#3264,#3264,#2806,.T.);
#3960=EDGE_CURVE('',#3261,#3263,#2004,.T.);
#3961=EDGE_CURVE('',#3264,#3265,#2005,.T.);
#3962=EDGE_CURVE('',#3265,#3265,#2807,.T.);
#3963=EDGE_CURVE('',#3266,#3266,#2808,.T.);
#3964=EDGE_CURVE('',#3266,#3262,#2006,.T.);
#3965=EDGE_CURVE('',#3267,#3267,#2809,.T.);
#3966=EDGE_CURVE('',#3267,#3268,#2007,.T.);
#3967=EDGE_CURVE('',#3268,#3268,#2810,.T.);
#3968=EDGE_CURVE('',#3269,#3269,#2811,.T.);
#3969=EDGE_CURVE('',#3269,#3270,#2008,.T.);
#3970=EDGE_CURVE('',#3270,#3270,#2812,.T.);
#3971=EDGE_CURVE('',#3271,#3272,#2009,.T.);
#3972=EDGE_CURVE('',#3271,#3272,#2813,.T.);
#3973=EDGE_CURVE('',#3273,#3271,#263,.T.);
#3974=EDGE_CURVE('',#3274,#3273,#2814,.T.);
#3975=EDGE_CURVE('',#3274,#3275,#2010,.T.);
#3976=EDGE_CURVE('',#3276,#3275,#264,.T.);
#3977=EDGE_CURVE('',#3275,#3276,#265,.T.);
#3978=EDGE_CURVE('',#3277,#3274,#2815,.T.);
#3979=EDGE_CURVE('',#3272,#3277,#266,.T.);
#3980=EDGE_CURVE('',#3277,#3273,#2011,.T.);
#3981=EDGE_CURVE('',#3278,#3278,#2816,.T.);
#3982=EDGE_CURVE('',#3278,#3279,#2012,.T.);
#3983=EDGE_CURVE('',#3279,#3279,#2817,.T.);
#3984=EDGE_CURVE('',#3280,#3280,#2818,.T.);
#3985=EDGE_CURVE('',#3280,#3281,#2013,.T.);
#3986=EDGE_CURVE('',#3281,#3281,#2819,.T.);
#3987=EDGE_CURVE('',#3282,#3283,#2014,.T.);
#3988=EDGE_CURVE('',#3282,#3283,#2820,.T.);
#3989=EDGE_CURVE('',#3284,#3282,#267,.T.);
#3990=EDGE_CURVE('',#3285,#3284,#2821,.T.);
#3991=EDGE_CURVE('',#3285,#3286,#2015,.T.);
#3992=EDGE_CURVE('',#3287,#3286,#268,.T.);
#3993=EDGE_CURVE('',#3286,#3287,#269,.T.);
#3994=EDGE_CURVE('',#3288,#3285,#2822,.T.);
#3995=EDGE_CURVE('',#3283,#3288,#270,.T.);
#3996=EDGE_CURVE('',#3288,#3284,#2016,.T.);
#3997=EDGE_CURVE('',#3289,#3290,#2017,.T.);
#3998=EDGE_CURVE('',#3291,#3289,#2018,.T.);
#3999=EDGE_CURVE('',#3291,#3292,#2019,.T.);
#4000=EDGE_CURVE('',#3292,#3290,#2020,.T.);
#4001=EDGE_CURVE('',#3290,#3293,#2021,.T.);
#4002=EDGE_CURVE('',#3292,#3294,#2022,.T.);
#4003=EDGE_CURVE('',#3294,#3295,#2023,.T.);
#4004=EDGE_CURVE('',#3296,#3295,#2024,.T.);
#4005=EDGE_CURVE('',#3293,#3296,#2025,.T.);
#4006=EDGE_CURVE('',#3297,#3289,#2026,.T.);
#4007=EDGE_CURVE('',#3298,#3297,#2027,.T.);
#4008=EDGE_CURVE('',#3299,#3298,#2028,.T.);
#4009=EDGE_CURVE('',#3300,#3299,#2029,.T.);
#4010=EDGE_CURVE('',#3300,#3291,#2030,.T.);
#4011=EDGE_CURVE('',#3295,#3299,#2031,.T.);
#4012=EDGE_CURVE('',#3294,#3300,#2032,.T.);
#4013=EDGE_CURVE('',#3301,#3301,#2823,.T.);
#4014=EDGE_CURVE('',#3293,#3297,#2824,.T.);
#4015=EDGE_CURVE('',#3302,#3303,#2033,.T.);
#4016=EDGE_CURVE('',#3302,#3304,#2034,.T.);
#4017=EDGE_CURVE('',#3305,#3304,#2035,.T.);
#4018=EDGE_CURVE('',#3303,#3305,#2036,.T.);
#4019=EDGE_CURVE('',#3303,#3306,#2037,.T.);
#4020=EDGE_CURVE('',#3307,#3305,#2038,.T.);
#4021=EDGE_CURVE('',#3306,#3307,#2039,.T.);
#4022=EDGE_CURVE('',#3306,#3308,#2040,.T.);
#4023=EDGE_CURVE('',#3309,#3307,#2041,.T.);
#4024=EDGE_CURVE('',#3308,#3309,#2042,.T.);
#4025=EDGE_CURVE('',#3308,#3302,#2043,.T.);
#4026=EDGE_CURVE('',#3304,#3309,#2044,.T.);
#4027=EDGE_CURVE('',#3296,#3298,#2825,.T.);
#4028=EDGE_CURVE('',#3310,#3310,#2826,.T.);
#4029=EDGE_CURVE('',#3301,#3310,#2045,.T.);
#4030=EDGE_CURVE('',#3311,#3312,#2046,.T.);
#4031=EDGE_CURVE('',#3311,#3312,#2827,.T.);
#4032=EDGE_CURVE('',#3313,#3311,#271,.T.);
#4033=EDGE_CURVE('',#3314,#3313,#2828,.T.);
#4034=EDGE_CURVE('',#3314,#3315,#2047,.T.);
#4035=EDGE_CURVE('',#3316,#3315,#272,.T.);
#4036=EDGE_CURVE('',#3315,#3316,#273,.T.);
#4037=EDGE_CURVE('',#3317,#3314,#2829,.T.);
#4038=EDGE_CURVE('',#3312,#3317,#274,.T.);
#4039=EDGE_CURVE('',#3317,#3313,#2048,.T.);
#4040=EDGE_CURVE('',#3318,#3319,#2049,.T.);
#4041=EDGE_CURVE('',#3318,#3320,#2050,.T.);
#4042=EDGE_CURVE('',#3321,#3320,#2051,.T.);
#4043=EDGE_CURVE('',#3319,#3321,#2052,.T.);
#4044=EDGE_CURVE('',#3322,#3318,#2053,.T.);
#4045=EDGE_CURVE('',#3322,#3323,#2054,.T.);
#4046=EDGE_CURVE('',#3320,#3323,#2055,.T.);
#4047=EDGE_CURVE('',#3324,#3322,#2056,.T.);
#4048=EDGE_CURVE('',#3325,#3324,#2057,.T.);
#4049=EDGE_CURVE('',#3323,#3325,#2058,.T.);
#4050=EDGE_CURVE('',#3326,#3326,#2830,.T.);
#4051=EDGE_CURVE('',#3325,#3321,#2831,.T.);
#4052=EDGE_CURVE('',#3324,#3319,#2832,.T.);
#4053=EDGE_CURVE('',#3327,#3327,#2833,.T.);
#4054=EDGE_CURVE('',#3327,#3328,#2059,.T.);
#4055=EDGE_CURVE('',#3328,#3328,#2834,.T.);
#4056=EDGE_CURVE('',#3329,#3330,#2060,.T.);
#4057=EDGE_CURVE('',#3331,#3329,#2835,.T.);
#4058=EDGE_CURVE('',#3332,#3331,#2061,.T.);
#4059=EDGE_CURVE('',#3332,#3330,#2836,.T.);
#4060=EDGE_CURVE('',#3332,#3333,#2062,.T.);
#4061=EDGE_CURVE('',#3334,#3333,#2837,.T.);
#4062=EDGE_CURVE('',#3334,#3330,#2063,.T.);
#4063=EDGE_CURVE('',#3335,#3331,#2064,.T.);
#4064=EDGE_CURVE('',#3333,#3335,#2065,.T.);
#4065=EDGE_CURVE('',#3329,#3336,#2066,.T.);
#4066=EDGE_CURVE('',#3335,#3336,#2838,.T.);
#4067=EDGE_CURVE('',#3336,#3334,#2067,.T.);
#4068=EDGE_CURVE('',#3326,#3337,#2068,.T.);
#4069=EDGE_CURVE('',#3337,#3337,#2839,.T.);
#4070=EDGE_CURVE('',#3338,#3338,#2840,.T.);
#4071=EDGE_CURVE('',#3338,#3339,#2069,.T.);
#4072=EDGE_CURVE('',#3339,#3339,#2841,.T.);
#4073=EDGE_CURVE('',#3340,#3340,#2842,.T.);
#4074=EDGE_CURVE('',#3340,#3341,#2070,.T.);
#4075=EDGE_CURVE('',#3341,#3341,#2843,.T.);
#4076=EDGE_CURVE('',#3342,#3342,#2844,.T.);
#4077=EDGE_CURVE('',#3342,#3343,#2071,.T.);
#4078=EDGE_CURVE('',#3343,#3343,#2845,.T.);
#4079=EDGE_CURVE('',#3344,#3344,#2846,.T.);
#4080=EDGE_CURVE('',#3344,#3345,#2072,.T.);
#4081=EDGE_CURVE('',#3345,#3345,#2847,.T.);
#4082=EDGE_CURVE('',#3346,#3346,#2848,.T.);
#4083=EDGE_CURVE('',#3347,#3347,#2849,.T.);
#4084=EDGE_CURVE('',#3347,#3346,#2073,.T.);
#4085=EDGE_CURVE('',#3348,#3348,#2850,.T.);
#4086=EDGE_CURVE('',#3348,#3349,#2074,.T.);
#4087=EDGE_CURVE('',#3349,#3349,#2851,.T.);
#4088=EDGE_CURVE('',#3350,#3351,#2075,.T.);
#4089=EDGE_CURVE('',#3352,#3350,#2076,.T.);
#4090=EDGE_CURVE('',#3353,#3352,#2077,.T.);
#4091=EDGE_CURVE('',#3354,#3353,#2078,.T.);
#4092=EDGE_CURVE('',#3355,#3354,#2079,.T.);
#4093=EDGE_CURVE('',#3356,#3355,#2080,.T.);
#4094=EDGE_CURVE('',#3357,#3356,#2081,.T.);
#4095=EDGE_CURVE('',#3351,#3357,#2082,.T.);
#4096=EDGE_CURVE('',#3354,#3358,#2083,.T.);
#4097=EDGE_CURVE('',#3358,#3359,#2084,.T.);
#4098=EDGE_CURVE('',#3359,#3355,#2085,.T.);
#4099=EDGE_CURVE('',#3360,#3353,#2086,.T.);
#4100=EDGE_CURVE('',#3360,#3358,#2087,.T.);
#4101=EDGE_CURVE('',#3352,#3361,#2088,.T.);
#4102=EDGE_CURVE('',#3361,#3360,#2089,.T.);
#4103=EDGE_CURVE('',#3362,#3350,#2090,.T.);
#4104=EDGE_CURVE('',#3362,#3361,#2091,.T.);
#4105=EDGE_CURVE('',#3363,#3362,#2092,.T.);
#4106=EDGE_CURVE('',#3364,#3363,#2093,.T.);
#4107=EDGE_CURVE('',#3365,#3364,#2094,.T.);
#4108=EDGE_CURVE('',#3359,#3365,#2095,.T.);
#4109=EDGE_CURVE('',#3351,#3363,#2096,.T.);
#4110=EDGE_CURVE('',#3364,#3357,#2097,.T.);
#4111=EDGE_CURVE('',#3356,#3365,#2098,.T.);
#4112=EDGE_CURVE('',#3366,#3367,#2099,.T.);
#4113=EDGE_CURVE('',#3366,#3368,#2100,.T.);
#4114=EDGE_CURVE('',#3368,#3369,#2101,.T.);
#4115=EDGE_CURVE('',#3367,#3369,#2102,.T.);
#4116=EDGE_CURVE('',#3370,#3366,#2103,.T.);
#4117=EDGE_CURVE('',#3370,#3371,#2104,.T.);
#4118=EDGE_CURVE('',#3371,#3368,#2105,.T.);
#4119=EDGE_CURVE('',#3372,#3370,#2106,.T.);
#4120=EDGE_CURVE('',#3372,#3373,#2107,.T.);
#4121=EDGE_CURVE('',#3373,#3371,#2108,.T.);
#4122=EDGE_CURVE('',#3374,#3372,#2109,.T.);
#4123=EDGE_CURVE('',#3374,#3375,#2110,.T.);
#4124=EDGE_CURVE('',#3375,#3373,#2111,.T.);
#4125=EDGE_CURVE('',#3376,#3374,#2112,.T.);
#4126=EDGE_CURVE('',#3376,#3377,#2113,.T.);
#4127=EDGE_CURVE('',#3377,#3375,#2114,.T.);
#4128=EDGE_CURVE('',#3367,#3376,#2115,.T.);
#4129=EDGE_CURVE('',#3369,#3377,#2116,.T.);
#4130=EDGE_CURVE('',#3378,#3378,#2852,.T.);
#4131=EDGE_CURVE('',#3379,#3379,#2853,.T.);
#4132=EDGE_CURVE('',#3379,#3378,#2117,.T.);
#4133=EDGE_CURVE('',#3380,#3380,#2854,.F.);
#4134=EDGE_CURVE('',#3380,#3379,#2118,.T.);
#4135=EDGE_CURVE('',#3381,#3381,#2855,.T.);
#4136=EDGE_CURVE('',#3381,#3380,#2119,.T.);
#4137=EDGE_CURVE('',#3382,#3383,#2856,.T.);
#4138=EDGE_CURVE('',#3383,#3382,#2857,.T.);
#4139=EDGE_CURVE('',#3383,#3384,#2858,.T.);
#4140=EDGE_CURVE('',#3385,#3384,#2859,.T.);
#4141=EDGE_CURVE('',#3384,#3385,#2860,.T.);
#4142=EDGE_CURVE('',#3385,#3386,#2120,.T.);
#4143=EDGE_CURVE('',#3386,#3386,#2861,.T.);
#4144=EDGE_CURVE('',#3387,#3387,#2862,.T.);
#4145=EDGE_CURVE('',#3387,#3388,#2121,.T.);
#4146=EDGE_CURVE('',#3388,#3388,#2863,.T.);
#4147=EDGE_CURVE('',#3388,#3389,#2122,.T.);
#4148=EDGE_CURVE('',#3389,#3389,#2864,.T.);
#4149=EDGE_CURVE('',#3390,#3390,#2865,.T.);
#4150=EDGE_CURVE('',#3390,#3382,#2123,.T.);
#4151=EDGE_CURVE('',#3391,#3391,#2866,.T.);
#4152=EDGE_CURVE('',#3391,#3387,#2124,.T.);
#4153=EDGE_CURVE('',#3392,#3393,#2867,.T.);
#4154=EDGE_CURVE('',#3393,#3392,#2868,.T.);
#4155=EDGE_CURVE('',#3393,#3394,#2869,.T.);
#4156=EDGE_CURVE('',#3395,#3394,#2870,.T.);
#4157=EDGE_CURVE('',#3394,#3395,#2871,.T.);
#4158=EDGE_CURVE('',#3396,#3396,#2872,.T.);
#4159=EDGE_CURVE('',#3396,#3395,#2125,.T.);
#4160=EDGE_CURVE('',#3397,#3397,#2873,.T.);
#4161=EDGE_CURVE('',#3398,#3398,#2874,.T.);
#4162=EDGE_CURVE('',#3399,#3399,#2875,.T.);
#4163=EDGE_CURVE('',#3399,#3397,#2126,.T.);
#4164=EDGE_CURVE('',#3400,#3400,#2876,.T.);
#4165=EDGE_CURVE('',#3400,#3399,#2127,.T.);
#4166=EDGE_CURVE('',#3401,#3401,#2877,.T.);
#4167=EDGE_CURVE('',#3401,#3400,#2128,.T.);
#4168=EDGE_CURVE('',#3392,#3398,#2129,.T.);
#4169=EDGE_CURVE('',#3402,#3403,#2878,.T.);
#4170=EDGE_CURVE('',#3404,#3405,#2879,.T.);
#4171=EDGE_CURVE('',#3406,#3407,#2880,.T.);
#4172=EDGE_CURVE('',#3408,#3409,#2881,.T.);
#4173=EDGE_CURVE('',#3410,#3411,#2882,.T.);
#4174=EDGE_CURVE('',#3412,#3413,#2883,.T.);
#4175=EDGE_CURVE('',#3414,#3415,#2884,.T.);
#4176=EDGE_CURVE('',#3416,#3417,#2885,.T.);
#4177=EDGE_CURVE('',#3418,#3419,#275,.T.);
#4178=EDGE_CURVE('',#3420,#3418,#2886,.T.);
#4179=EDGE_CURVE('',#3421,#3420,#276,.T.);
#4180=EDGE_CURVE('',#3419,#3421,#2887,.T.);
#4181=EDGE_CURVE('',#3422,#3420,#2888,.T.);
#4182=EDGE_CURVE('',#3422,#3423,#277,.T.);
#4183=EDGE_CURVE('',#3424,#3423,#2889,.T.);
#4184=EDGE_CURVE('',#3424,#3425,#278,.T.);
#4185=EDGE_CURVE('',#3426,#3425,#2890,.T.);
#4186=EDGE_CURVE('',#3426,#3427,#279,.T.);
#4187=EDGE_CURVE('',#3427,#3428,#2130,.T.);
#4188=EDGE_CURVE('',#3428,#3428,#2891,.T.);
#4189=EDGE_CURVE('',#3427,#3429,#280,.T.);
#4190=EDGE_CURVE('',#3430,#3429,#2892,.T.);
#4191=EDGE_CURVE('',#3430,#3431,#281,.T.);
#4192=EDGE_CURVE('',#3432,#3431,#2893,.T.);
#4193=EDGE_CURVE('',#3432,#3433,#282,.T.);
#4194=EDGE_CURVE('',#3434,#3433,#2894,.T.);
#4195=EDGE_CURVE('',#3434,#3435,#283,.T.);
#4196=EDGE_CURVE('',#3436,#3435,#2895,.T.);
#4197=EDGE_CURVE('',#3436,#3437,#284,.T.);
#4198=EDGE_CURVE('',#3421,#3437,#2896,.T.);
#4199=EDGE_CURVE('',#3418,#3438,#2897,.T.);
#4200=EDGE_CURVE('',#3438,#3422,#2898,.T.);
#4201=EDGE_CURVE('',#3439,#3438,#285,.T.);
#4202=EDGE_CURVE('',#3423,#3439,#2899,.T.);
#4203=EDGE_CURVE('',#3439,#3440,#2900,.T.);
#4204=EDGE_CURVE('',#3440,#3424,#2901,.T.);
#4205=EDGE_CURVE('',#3441,#3440,#286,.T.);
#4206=EDGE_CURVE('',#3425,#3441,#2902,.T.);
#4207=EDGE_CURVE('',#3441,#3442,#2903,.T.);
#4208=EDGE_CURVE('',#3442,#3426,#2904,.T.);
#4209=EDGE_CURVE('',#3443,#3444,#287,.T.);
#4210=EDGE_CURVE('',#3429,#3443,#2905,.T.);
#4211=EDGE_CURVE('',#3444,#3442,#288,.T.);
#4212=EDGE_CURVE('',#3443,#3445,#2906,.T.);
#4213=EDGE_CURVE('',#3445,#3430,#2907,.T.);
#4214=EDGE_CURVE('',#3446,#3445,#289,.T.);
#4215=EDGE_CURVE('',#3431,#3446,#2908,.T.);
#4216=EDGE_CURVE('',#3446,#3447,#2909,.T.);
#4217=EDGE_CURVE('',#3447,#3432,#2910,.T.);
#4218=EDGE_CURVE('',#3448,#3447,#290,.T.);
#4219=EDGE_CURVE('',#3433,#3448,#2911,.T.);
#4220=EDGE_CURVE('',#3448,#3449,#2912,.T.);
#4221=EDGE_CURVE('',#3449,#3434,#2913,.T.);
#4222=EDGE_CURVE('',#3450,#3449,#291,.T.);
#4223=EDGE_CURVE('',#3435,#3450,#2914,.T.);
#4224=EDGE_CURVE('',#3451,#3451,#2915,.T.);
#4225=EDGE_CURVE('',#3451,#3444,#2131,.T.);
#4226=EDGE_CURVE('',#3452,#3419,#2916,.T.);
#4227=EDGE_CURVE('',#3452,#3453,#292,.T.);
#4228=EDGE_CURVE('',#3450,#3453,#2917,.T.);
#4229=EDGE_CURVE('',#3437,#3452,#2918,.T.);
#4230=EDGE_CURVE('',#3453,#3436,#2919,.T.);
#4231=EDGE_CURVE('',#3454,#3454,#2920,.T.);
#4232=EDGE_CURVE('',#3455,#3455,#2921,.T.);
#4233=EDGE_CURVE('',#3456,#3456,#2922,.T.);
#4234=EDGE_CURVE('',#3456,#3454,#2132,.T.);
#4235=EDGE_CURVE('',#3457,#3457,#2923,.T.);
#4236=EDGE_CURVE('',#3457,#3455,#2133,.T.);
#4237=EDGE_CURVE('',#3458,#3458,#2924,.T.);
#4238=EDGE_CURVE('',#3459,#3459,#2925,.T.);
#4239=EDGE_CURVE('',#3460,#3460,#2926,.T.);
#4240=EDGE_CURVE('',#3460,#3458,#2134,.T.);
#4241=EDGE_CURVE('',#3461,#3461,#2927,.T.);
#4242=EDGE_CURVE('',#3461,#3459,#2135,.T.);
#4243=EDGE_CURVE('',#3462,#3462,#2928,.T.);
#4244=EDGE_CURVE('',#3462,#3463,#2136,.T.);
#4245=EDGE_CURVE('',#3463,#3463,#2929,.T.);
#4246=EDGE_CURVE('',#3464,#3464,#2930,.T.);
#4247=EDGE_CURVE('',#3464,#3465,#2137,.T.);
#4248=EDGE_CURVE('',#3465,#3465,#2931,.T.);
#4249=EDGE_CURVE('',#3466,#3466,#2932,.T.);
#4250=EDGE_CURVE('',#3466,#3467,#2138,.T.);
#4251=EDGE_CURVE('',#3467,#3467,#2933,.T.);
#4252=EDGE_CURVE('',#3468,#3469,#2139,.T.);
#4253=EDGE_CURVE('',#3468,#3470,#2140,.T.);
#4254=EDGE_CURVE('',#3471,#3470,#2141,.T.);
#4255=EDGE_CURVE('',#3469,#3471,#2142,.T.);
#4256=EDGE_CURVE('',#3472,#3473,#2143,.T.);
#4257=EDGE_CURVE('',#3472,#3474,#2144,.T.);
#4258=EDGE_CURVE('',#3475,#3474,#2145,.T.);
#4259=EDGE_CURVE('',#3473,#3475,#2146,.T.);
#4260=EDGE_CURVE('',#3474,#3476,#2147,.T.);
#4261=EDGE_CURVE('',#3476,#3477,#2148,.T.);
#4262=EDGE_CURVE('',#3477,#3475,#2149,.T.);
#4263=EDGE_CURVE('',#3470,#3472,#2150,.T.);
#4264=EDGE_CURVE('',#3473,#3471,#2151,.T.);
#4265=EDGE_CURVE('',#3469,#3478,#2152,.T.);
#4266=EDGE_CURVE('',#3478,#3479,#2153,.T.);
#4267=EDGE_CURVE('',#3479,#3468,#2154,.T.);
#4268=EDGE_CURVE('',#3480,#3481,#2155,.T.);
#4269=EDGE_CURVE('',#3480,#3478,#2156,.T.);
#4270=EDGE_CURVE('',#3481,#3477,#2157,.T.);
#4271=EDGE_CURVE('',#3481,#3482,#2158,.T.);
#4272=EDGE_CURVE('',#3482,#3476,#2159,.T.);
#4273=EDGE_CURVE('',#3482,#3483,#2160,.T.);
#4274=EDGE_CURVE('',#3483,#3479,#2161,.T.);
#4275=EDGE_CURVE('',#3483,#3480,#2162,.T.);
#4276=EDGE_CURVE('',#3484,#3484,#2934,.T.);
#4277=EDGE_CURVE('',#3484,#3485,#2163,.T.);
#4278=EDGE_CURVE('',#3485,#3485,#2935,.T.);
#4279=EDGE_CURVE('',#3486,#3486,#2936,.T.);
#4280=EDGE_CURVE('',#3486,#3487,#2164,.T.);
#4281=EDGE_CURVE('',#3487,#3487,#2937,.T.);
#4282=EDGE_CURVE('',#3488,#3488,#2938,.T.);
#4283=EDGE_CURVE('',#3488,#3489,#2165,.T.);
#4284=EDGE_CURVE('',#3489,#3489,#2939,.T.);
#4285=EDGE_CURVE('',#3490,#3490,#2940,.T.);
#4286=EDGE_CURVE('',#3490,#3491,#2166,.T.);
#4287=EDGE_CURVE('',#3491,#3491,#2941,.T.);
#4288=EDGE_CURVE('',#3492,#3492,#2942,.T.);
#4289=EDGE_CURVE('',#3492,#3493,#2167,.T.);
#4290=EDGE_CURVE('',#3493,#3493,#2943,.T.);
#4291=EDGE_CURVE('',#3494,#3494,#2944,.T.);
#4292=EDGE_CURVE('',#3494,#3495,#2168,.T.);
#4293=EDGE_CURVE('',#3495,#3495,#2945,.T.);
#4294=EDGE_CURVE('',#3496,#3496,#2946,.T.);
#4295=EDGE_CURVE('',#3496,#3497,#2169,.T.);
#4296=EDGE_CURVE('',#3497,#3497,#2947,.T.);
#4297=EDGE_CURVE('',#3498,#3498,#2948,.T.);
#4298=EDGE_CURVE('',#3498,#3499,#2170,.T.);
#4299=EDGE_CURVE('',#3499,#3499,#2949,.T.);
#4300=EDGE_CURVE('',#3500,#3500,#2950,.T.);
#4301=EDGE_CURVE('',#3500,#3501,#2171,.T.);
#4302=EDGE_CURVE('',#3501,#3501,#2951,.T.);
#4303=EDGE_CURVE('',#3502,#3502,#2952,.T.);
#4304=EDGE_CURVE('',#3502,#3503,#2172,.T.);
#4305=EDGE_CURVE('',#3503,#3503,#2953,.T.);
#4306=EDGE_CURVE('',#3504,#3504,#2954,.T.);
#4307=EDGE_CURVE('',#3504,#3505,#2173,.T.);
#4308=EDGE_CURVE('',#3505,#3505,#2955,.T.);
#4309=EDGE_CURVE('',#3506,#3506,#2956,.T.);
#4310=EDGE_CURVE('',#3506,#3507,#2174,.T.);
#4311=EDGE_CURVE('',#3507,#3507,#2957,.T.);
#4312=EDGE_CURVE('',#3508,#3508,#2958,.T.);
#4313=EDGE_CURVE('',#3508,#3509,#2175,.T.);
#4314=EDGE_CURVE('',#3509,#3509,#2959,.T.);
#4315=EDGE_CURVE('',#3510,#3510,#2960,.T.);
#4316=EDGE_CURVE('',#3510,#3511,#2176,.T.);
#4317=EDGE_CURVE('',#3511,#3511,#2961,.T.);
#4318=EDGE_CURVE('',#3512,#3512,#2962,.T.);
#4319=EDGE_CURVE('',#3512,#3513,#2177,.T.);
#4320=EDGE_CURVE('',#3513,#3513,#2963,.T.);
#4321=EDGE_CURVE('',#3514,#3515,#2178,.T.);
#4322=EDGE_CURVE('',#3515,#3516,#2179,.T.);
#4323=EDGE_CURVE('',#3516,#3517,#2180,.T.);
#4324=EDGE_CURVE('',#3514,#3517,#2181,.T.);
#4325=EDGE_CURVE('',#3515,#3518,#2182,.T.);
#4326=EDGE_CURVE('',#3518,#3519,#2183,.T.);
#4327=EDGE_CURVE('',#3519,#3516,#2184,.T.);
#4328=EDGE_CURVE('',#3518,#3520,#2185,.T.);
#4329=EDGE_CURVE('',#3520,#3521,#2186,.T.);
#4330=EDGE_CURVE('',#3521,#3519,#2187,.T.);
#4331=EDGE_CURVE('',#3520,#3522,#2188,.T.);
#4332=EDGE_CURVE('',#3522,#3523,#2189,.T.);
#4333=EDGE_CURVE('',#3523,#3521,#2190,.T.);
#4334=EDGE_CURVE('',#3522,#3524,#2191,.T.);
#4335=EDGE_CURVE('',#3524,#3525,#2192,.T.);
#4336=EDGE_CURVE('',#3525,#3523,#2193,.T.);
#4337=EDGE_CURVE('',#3524,#3514,#2194,.T.);
#4338=EDGE_CURVE('',#3517,#3525,#2195,.T.);
#4339=EDGE_CURVE('',#3526,#3526,#2964,.T.);
#4340=EDGE_CURVE('',#3527,#3527,#2965,.T.);
#4341=EDGE_CURVE('',#3528,#3528,#2966,.T.);
#4342=EDGE_CURVE('',#3528,#3527,#2196,.T.);
#4343=EDGE_CURVE('',#3529,#3529,#2967,.T.);
#4344=EDGE_CURVE('',#3529,#3528,#2197,.T.);
#4345=EDGE_CURVE('',#3530,#3530,#2968,.T.);
#4346=EDGE_CURVE('',#3530,#3529,#2198,.T.);
#4347=EDGE_CURVE('',#3531,#3531,#2969,.T.);
#4348=EDGE_CURVE('',#3532,#3532,#2970,.F.);
#4349=EDGE_CURVE('',#3532,#3531,#2199,.T.);
#4350=EDGE_CURVE('',#3526,#3532,#2200,.T.);
#4351=ORIENTED_EDGE('',*,*,#3533,.F.);
#4352=ORIENTED_EDGE('',*,*,#3534,.T.);
#4353=ORIENTED_EDGE('',*,*,#3535,.F.);
#4354=ORIENTED_EDGE('',*,*,#3534,.F.);
#4355=ORIENTED_EDGE('',*,*,#3536,.F.);
#4356=ORIENTED_EDGE('',*,*,#3537,.T.);
#4357=ORIENTED_EDGE('',*,*,#3538,.F.);
#4358=ORIENTED_EDGE('',*,*,#3537,.F.);
#4359=ORIENTED_EDGE('',*,*,#3539,.F.);
#4360=ORIENTED_EDGE('',*,*,#3540,.T.);
#4361=ORIENTED_EDGE('',*,*,#3541,.F.);
#4362=ORIENTED_EDGE('',*,*,#3540,.F.);
#4363=ORIENTED_EDGE('',*,*,#3542,.F.);
#4364=ORIENTED_EDGE('',*,*,#3543,.T.);
#4365=ORIENTED_EDGE('',*,*,#3544,.F.);
#4366=ORIENTED_EDGE('',*,*,#3543,.F.);
#4367=ORIENTED_EDGE('',*,*,#3545,.T.);
#4368=ORIENTED_EDGE('',*,*,#3546,.T.);
#4369=ORIENTED_EDGE('',*,*,#3547,.F.);
#4370=ORIENTED_EDGE('',*,*,#3548,.F.);
#4371=ORIENTED_EDGE('',*,*,#3549,.T.);
#4372=ORIENTED_EDGE('',*,*,#3548,.T.);
#4373=ORIENTED_EDGE('',*,*,#3550,.F.);
#4374=ORIENTED_EDGE('',*,*,#3551,.F.);
#4375=ORIENTED_EDGE('',*,*,#3552,.T.);
#4376=ORIENTED_EDGE('',*,*,#3551,.T.);
#4377=ORIENTED_EDGE('',*,*,#3553,.F.);
#4378=ORIENTED_EDGE('',*,*,#3554,.F.);
#4379=ORIENTED_EDGE('',*,*,#3555,.T.);
#4380=ORIENTED_EDGE('',*,*,#3554,.T.);
#4381=ORIENTED_EDGE('',*,*,#3556,.F.);
#4382=ORIENTED_EDGE('',*,*,#3546,.F.);
#4383=ORIENTED_EDGE('',*,*,#3556,.T.);
#4384=ORIENTED_EDGE('',*,*,#3553,.T.);
#4385=ORIENTED_EDGE('',*,*,#3550,.T.);
#4386=ORIENTED_EDGE('',*,*,#3547,.T.);
#4387=ORIENTED_EDGE('',*,*,#3535,.T.);
#4388=ORIENTED_EDGE('',*,*,#3538,.T.);
#4389=ORIENTED_EDGE('',*,*,#3541,.T.);
#4390=ORIENTED_EDGE('',*,*,#3544,.T.);
#4391=ORIENTED_EDGE('',*,*,#3555,.F.);
#4392=ORIENTED_EDGE('',*,*,#3545,.F.);
#4393=ORIENTED_EDGE('',*,*,#3549,.F.);
#4394=ORIENTED_EDGE('',*,*,#3552,.F.);
#4395=ORIENTED_EDGE('',*,*,#3533,.T.);
#4396=ORIENTED_EDGE('',*,*,#3536,.T.);
#4397=ORIENTED_EDGE('',*,*,#3539,.T.);
#4398=ORIENTED_EDGE('',*,*,#3542,.T.);
#4399=ORIENTED_EDGE('',*,*,#3557,.F.);
#4400=ORIENTED_EDGE('',*,*,#3558,.T.);
#4401=ORIENTED_EDGE('',*,*,#3559,.F.);
#4402=ORIENTED_EDGE('',*,*,#3558,.F.);
#4403=ORIENTED_EDGE('',*,*,#3557,.T.);
#4404=ORIENTED_EDGE('',*,*,#3560,.F.);
#4405=ORIENTED_EDGE('',*,*,#3561,.T.);
#4406=ORIENTED_EDGE('',*,*,#3562,.F.);
#4407=ORIENTED_EDGE('',*,*,#3561,.F.);
#4408=ORIENTED_EDGE('',*,*,#3560,.T.);
#4409=ORIENTED_EDGE('',*,*,#3563,.F.);
#4410=ORIENTED_EDGE('',*,*,#3564,.T.);
#4411=ORIENTED_EDGE('',*,*,#3565,.F.);
#4412=ORIENTED_EDGE('',*,*,#3564,.F.);
#4413=ORIENTED_EDGE('',*,*,#3563,.T.);
#4414=ORIENTED_EDGE('',*,*,#3566,.F.);
#4415=ORIENTED_EDGE('',*,*,#3567,.T.);
#4416=ORIENTED_EDGE('',*,*,#3568,.F.);
#4417=ORIENTED_EDGE('',*,*,#3567,.F.);
#4418=ORIENTED_EDGE('',*,*,#3566,.T.);
#4419=ORIENTED_EDGE('',*,*,#3569,.F.);
#4420=ORIENTED_EDGE('',*,*,#3570,.T.);
#4421=ORIENTED_EDGE('',*,*,#3571,.T.);
#4422=ORIENTED_EDGE('',*,*,#3570,.F.);
#4423=ORIENTED_EDGE('',*,*,#3571,.F.);
#4424=ORIENTED_EDGE('',*,*,#3572,.F.);
#4425=ORIENTED_EDGE('',*,*,#3573,.T.);
#4426=ORIENTED_EDGE('',*,*,#3574,.T.);
#4427=ORIENTED_EDGE('',*,*,#3573,.F.);
#4428=ORIENTED_EDGE('',*,*,#3574,.F.);
#4429=ORIENTED_EDGE('',*,*,#3575,.F.);
#4430=ORIENTED_EDGE('',*,*,#3576,.T.);
#4431=ORIENTED_EDGE('',*,*,#3577,.T.);
#4432=ORIENTED_EDGE('',*,*,#3576,.F.);
#4433=ORIENTED_EDGE('',*,*,#3577,.F.);
#4434=ORIENTED_EDGE('',*,*,#3578,.F.);
#4435=ORIENTED_EDGE('',*,*,#3579,.T.);
#4436=ORIENTED_EDGE('',*,*,#3580,.T.);
#4437=ORIENTED_EDGE('',*,*,#3579,.F.);
#4438=ORIENTED_EDGE('',*,*,#3580,.F.);
#4439=ORIENTED_EDGE('',*,*,#3581,.F.);
#4440=ORIENTED_EDGE('',*,*,#3582,.F.);
#4441=ORIENTED_EDGE('',*,*,#3583,.F.);
#4442=ORIENTED_EDGE('',*,*,#3584,.F.);
#4443=ORIENTED_EDGE('',*,*,#3585,.F.);
#4444=ORIENTED_EDGE('',*,*,#3586,.F.);
#4445=ORIENTED_EDGE('',*,*,#3587,.F.);
#4446=ORIENTED_EDGE('',*,*,#3588,.F.);
#4447=ORIENTED_EDGE('',*,*,#3589,.F.);
#4448=ORIENTED_EDGE('',*,*,#3584,.T.);
#4449=ORIENTED_EDGE('',*,*,#3590,.F.);
#4450=ORIENTED_EDGE('',*,*,#3586,.T.);
#4451=ORIENTED_EDGE('',*,*,#3591,.F.);
#4452=ORIENTED_EDGE('',*,*,#3592,.F.);
#4453=ORIENTED_EDGE('',*,*,#3593,.F.);
#4454=ORIENTED_EDGE('',*,*,#3594,.F.);
#4455=ORIENTED_EDGE('',*,*,#3595,.F.);
#4456=ORIENTED_EDGE('',*,*,#3596,.F.);
#4457=ORIENTED_EDGE('',*,*,#3597,.F.);
#4458=ORIENTED_EDGE('',*,*,#3598,.F.);
#4459=ORIENTED_EDGE('',*,*,#3599,.F.);
#4460=ORIENTED_EDGE('',*,*,#3600,.F.);
#4461=ORIENTED_EDGE('',*,*,#3595,.T.);
#4462=ORIENTED_EDGE('',*,*,#3601,.F.);
#4463=ORIENTED_EDGE('',*,*,#3597,.T.);
#4464=ORIENTED_EDGE('',*,*,#3602,.F.);
#4465=ORIENTED_EDGE('',*,*,#3603,.F.);
#4466=ORIENTED_EDGE('',*,*,#3604,.F.);
#4467=ORIENTED_EDGE('',*,*,#3605,.F.);
#4468=ORIENTED_EDGE('',*,*,#3606,.F.);
#4469=ORIENTED_EDGE('',*,*,#3607,.F.);
#4470=ORIENTED_EDGE('',*,*,#3608,.F.);
#4471=ORIENTED_EDGE('',*,*,#3609,.F.);
#4472=ORIENTED_EDGE('',*,*,#3610,.F.);
#4473=ORIENTED_EDGE('',*,*,#3611,.F.);
#4474=ORIENTED_EDGE('',*,*,#3606,.T.);
#4475=ORIENTED_EDGE('',*,*,#3612,.F.);
#4476=ORIENTED_EDGE('',*,*,#3608,.T.);
#4477=ORIENTED_EDGE('',*,*,#3613,.F.);
#4478=ORIENTED_EDGE('',*,*,#3614,.F.);
#4479=ORIENTED_EDGE('',*,*,#3615,.F.);
#4480=ORIENTED_EDGE('',*,*,#3616,.F.);
#4481=ORIENTED_EDGE('',*,*,#3617,.F.);
#4482=ORIENTED_EDGE('',*,*,#3618,.F.);
#4483=ORIENTED_EDGE('',*,*,#3619,.F.);
#4484=ORIENTED_EDGE('',*,*,#3620,.F.);
#4485=ORIENTED_EDGE('',*,*,#3621,.F.);
#4486=ORIENTED_EDGE('',*,*,#3622,.F.);
#4487=ORIENTED_EDGE('',*,*,#3617,.T.);
#4488=ORIENTED_EDGE('',*,*,#3623,.F.);
#4489=ORIENTED_EDGE('',*,*,#3619,.T.);
#4490=ORIENTED_EDGE('',*,*,#3624,.F.);
#4491=ORIENTED_EDGE('',*,*,#3582,.T.);
#4492=ORIENTED_EDGE('',*,*,#3625,.F.);
#4493=ORIENTED_EDGE('',*,*,#3626,.T.);
#4494=ORIENTED_EDGE('',*,*,#3627,.F.);
#4495=ORIENTED_EDGE('',*,*,#3588,.T.);
#4496=ORIENTED_EDGE('',*,*,#3628,.F.);
#4497=ORIENTED_EDGE('',*,*,#3629,.F.);
#4498=ORIENTED_EDGE('',*,*,#3630,.F.);
#4499=ORIENTED_EDGE('',*,*,#3593,.T.);
#4500=ORIENTED_EDGE('',*,*,#3631,.F.);
#4501=ORIENTED_EDGE('',*,*,#3632,.F.);
#4502=ORIENTED_EDGE('',*,*,#3633,.F.);
#4503=ORIENTED_EDGE('',*,*,#3599,.T.);
#4504=ORIENTED_EDGE('',*,*,#3634,.F.);
#4505=ORIENTED_EDGE('',*,*,#3635,.F.);
#4506=ORIENTED_EDGE('',*,*,#3636,.F.);
#4507=ORIENTED_EDGE('',*,*,#3587,.T.);
#4508=ORIENTED_EDGE('',*,*,#3590,.T.);
#4509=ORIENTED_EDGE('',*,*,#3583,.T.);
#4510=ORIENTED_EDGE('',*,*,#3627,.T.);
#4511=ORIENTED_EDGE('',*,*,#3637,.T.);
#4512=ORIENTED_EDGE('',*,*,#3638,.T.);
#4513=ORIENTED_EDGE('',*,*,#3639,.T.);
#4514=ORIENTED_EDGE('',*,*,#3640,.T.);
#4515=ORIENTED_EDGE('',*,*,#3609,.T.);
#4516=ORIENTED_EDGE('',*,*,#3612,.T.);
#4517=ORIENTED_EDGE('',*,*,#3605,.T.);
#4518=ORIENTED_EDGE('',*,*,#3641,.T.);
#4519=ORIENTED_EDGE('',*,*,#3642,.F.);
#4520=ORIENTED_EDGE('',*,*,#3628,.T.);
#4521=ORIENTED_EDGE('',*,*,#3604,.T.);
#4522=ORIENTED_EDGE('',*,*,#3643,.F.);
#4523=ORIENTED_EDGE('',*,*,#3644,.F.);
#4524=ORIENTED_EDGE('',*,*,#3641,.F.);
#4525=ORIENTED_EDGE('',*,*,#3610,.T.);
#4526=ORIENTED_EDGE('',*,*,#3640,.F.);
#4527=ORIENTED_EDGE('',*,*,#3645,.F.);
#4528=ORIENTED_EDGE('',*,*,#3646,.F.);
#4529=ORIENTED_EDGE('',*,*,#3598,.T.);
#4530=ORIENTED_EDGE('',*,*,#3601,.T.);
#4531=ORIENTED_EDGE('',*,*,#3594,.T.);
#4532=ORIENTED_EDGE('',*,*,#3633,.T.);
#4533=ORIENTED_EDGE('',*,*,#3647,.F.);
#4534=ORIENTED_EDGE('',*,*,#3648,.T.);
#4535=ORIENTED_EDGE('',*,*,#3620,.T.);
#4536=ORIENTED_EDGE('',*,*,#3623,.T.);
#4537=ORIENTED_EDGE('',*,*,#3616,.T.);
#4538=ORIENTED_EDGE('',*,*,#3649,.T.);
#4539=ORIENTED_EDGE('',*,*,#3650,.T.);
#4540=ORIENTED_EDGE('',*,*,#3651,.T.);
#4541=ORIENTED_EDGE('',*,*,#3652,.T.);
#4542=ORIENTED_EDGE('',*,*,#3634,.T.);
#4543=ORIENTED_EDGE('',*,*,#3615,.T.);
#4544=ORIENTED_EDGE('',*,*,#3653,.F.);
#4545=ORIENTED_EDGE('',*,*,#3654,.T.);
#4546=ORIENTED_EDGE('',*,*,#3649,.F.);
#4547=ORIENTED_EDGE('',*,*,#3621,.T.);
#4548=ORIENTED_EDGE('',*,*,#3648,.F.);
#4549=ORIENTED_EDGE('',*,*,#3655,.F.);
#4550=ORIENTED_EDGE('',*,*,#3656,.F.);
#4551=ORIENTED_EDGE('',*,*,#3657,.F.);
#4552=ORIENTED_EDGE('',*,*,#3658,.T.);
#4553=ORIENTED_EDGE('',*,*,#3591,.T.);
#4554=ORIENTED_EDGE('',*,*,#3658,.F.);
#4555=ORIENTED_EDGE('',*,*,#3659,.F.);
#4556=ORIENTED_EDGE('',*,*,#3660,.T.);
#4557=ORIENTED_EDGE('',*,*,#3602,.T.);
#4558=ORIENTED_EDGE('',*,*,#3660,.F.);
#4559=ORIENTED_EDGE('',*,*,#3661,.F.);
#4560=ORIENTED_EDGE('',*,*,#3662,.T.);
#4561=ORIENTED_EDGE('',*,*,#3613,.T.);
#4562=ORIENTED_EDGE('',*,*,#3662,.F.);
#4563=ORIENTED_EDGE('',*,*,#3663,.F.);
#4564=ORIENTED_EDGE('',*,*,#3664,.T.);
#4565=ORIENTED_EDGE('',*,*,#3624,.T.);
#4566=ORIENTED_EDGE('',*,*,#3664,.F.);
#4567=ORIENTED_EDGE('',*,*,#3665,.F.);
#4568=ORIENTED_EDGE('',*,*,#3635,.T.);
#4569=ORIENTED_EDGE('',*,*,#3652,.F.);
#4570=ORIENTED_EDGE('',*,*,#3666,.F.);
#4571=ORIENTED_EDGE('',*,*,#3667,.F.);
#4572=ORIENTED_EDGE('',*,*,#3666,.T.);
#4573=ORIENTED_EDGE('',*,*,#3651,.F.);
#4574=ORIENTED_EDGE('',*,*,#3668,.F.);
#4575=ORIENTED_EDGE('',*,*,#3659,.T.);
#4576=ORIENTED_EDGE('',*,*,#3663,.T.);
#4577=ORIENTED_EDGE('',*,*,#3669,.F.);
#4578=ORIENTED_EDGE('',*,*,#3668,.T.);
#4579=ORIENTED_EDGE('',*,*,#3650,.F.);
#4580=ORIENTED_EDGE('',*,*,#3654,.F.);
#4581=ORIENTED_EDGE('',*,*,#3596,.T.);
#4582=ORIENTED_EDGE('',*,*,#3636,.T.);
#4583=ORIENTED_EDGE('',*,*,#3665,.T.);
#4584=ORIENTED_EDGE('',*,*,#3667,.T.);
#4585=ORIENTED_EDGE('',*,*,#3669,.T.);
#4586=ORIENTED_EDGE('',*,*,#3653,.T.);
#4587=ORIENTED_EDGE('',*,*,#3614,.T.);
#4588=ORIENTED_EDGE('',*,*,#3622,.T.);
#4589=ORIENTED_EDGE('',*,*,#3618,.T.);
#4590=ORIENTED_EDGE('',*,*,#3656,.T.);
#4591=ORIENTED_EDGE('',*,*,#3670,.F.);
#4592=ORIENTED_EDGE('',*,*,#3631,.T.);
#4593=ORIENTED_EDGE('',*,*,#3592,.T.);
#4594=ORIENTED_EDGE('',*,*,#3600,.T.);
#4595=ORIENTED_EDGE('',*,*,#3671,.F.);
#4596=ORIENTED_EDGE('',*,*,#3645,.T.);
#4597=ORIENTED_EDGE('',*,*,#3639,.F.);
#4598=ORIENTED_EDGE('',*,*,#3672,.F.);
#4599=ORIENTED_EDGE('',*,*,#3673,.F.);
#4600=ORIENTED_EDGE('',*,*,#3672,.T.);
#4601=ORIENTED_EDGE('',*,*,#3638,.F.);
#4602=ORIENTED_EDGE('',*,*,#3674,.F.);
#4603=ORIENTED_EDGE('',*,*,#3657,.T.);
#4604=ORIENTED_EDGE('',*,*,#3661,.T.);
#4605=ORIENTED_EDGE('',*,*,#3675,.F.);
#4606=ORIENTED_EDGE('',*,*,#3674,.T.);
#4607=ORIENTED_EDGE('',*,*,#3637,.F.);
#4608=ORIENTED_EDGE('',*,*,#3626,.F.);
#4609=ORIENTED_EDGE('',*,*,#3585,.T.);
#4610=ORIENTED_EDGE('',*,*,#3630,.T.);
#4611=ORIENTED_EDGE('',*,*,#3676,.F.);
#4612=ORIENTED_EDGE('',*,*,#3643,.T.);
#4613=ORIENTED_EDGE('',*,*,#3603,.T.);
#4614=ORIENTED_EDGE('',*,*,#3611,.T.);
#4615=ORIENTED_EDGE('',*,*,#3607,.T.);
#4616=ORIENTED_EDGE('',*,*,#3646,.T.);
#4617=ORIENTED_EDGE('',*,*,#3671,.T.);
#4618=ORIENTED_EDGE('',*,*,#3673,.T.);
#4619=ORIENTED_EDGE('',*,*,#3675,.T.);
#4620=ORIENTED_EDGE('',*,*,#3625,.T.);
#4621=ORIENTED_EDGE('',*,*,#3581,.T.);
#4622=ORIENTED_EDGE('',*,*,#3589,.T.);
#4623=ORIENTED_EDGE('',*,*,#3677,.F.);
#4624=ORIENTED_EDGE('',*,*,#3678,.T.);
#4625=ORIENTED_EDGE('',*,*,#3679,.T.);
#4626=ORIENTED_EDGE('',*,*,#3678,.F.);
#4627=ORIENTED_EDGE('',*,*,#3680,.F.);
#4628=ORIENTED_EDGE('',*,*,#3681,.T.);
#4629=ORIENTED_EDGE('',*,*,#3682,.T.);
#4630=ORIENTED_EDGE('',*,*,#3681,.F.);
#4631=ORIENTED_EDGE('',*,*,#3655,.T.);
#4632=ORIENTED_EDGE('',*,*,#3647,.T.);
#4633=ORIENTED_EDGE('',*,*,#3632,.T.);
#4634=ORIENTED_EDGE('',*,*,#3670,.T.);
#4635=ORIENTED_EDGE('',*,*,#3629,.T.);
#4636=ORIENTED_EDGE('',*,*,#3642,.T.);
#4637=ORIENTED_EDGE('',*,*,#3644,.T.);
#4638=ORIENTED_EDGE('',*,*,#3676,.T.);
#4639=ORIENTED_EDGE('',*,*,#3680,.T.);
#4640=ORIENTED_EDGE('',*,*,#3677,.T.);
#4641=ORIENTED_EDGE('',*,*,#3568,.T.);
#4642=ORIENTED_EDGE('',*,*,#3565,.T.);
#4643=ORIENTED_EDGE('',*,*,#3562,.T.);
#4644=ORIENTED_EDGE('',*,*,#3559,.T.);
#4645=ORIENTED_EDGE('',*,*,#3682,.F.);
#4646=ORIENTED_EDGE('',*,*,#3679,.F.);
#4647=ORIENTED_EDGE('',*,*,#3578,.T.);
#4648=ORIENTED_EDGE('',*,*,#3575,.T.);
#4649=ORIENTED_EDGE('',*,*,#3572,.T.);
#4650=ORIENTED_EDGE('',*,*,#3569,.T.);
#4651=ORIENTED_EDGE('',*,*,#3683,.F.);
#4652=ORIENTED_EDGE('',*,*,#3684,.T.);
#4653=ORIENTED_EDGE('',*,*,#3685,.T.);
#4654=ORIENTED_EDGE('',*,*,#3684,.F.);
#4655=ORIENTED_EDGE('',*,*,#3686,.F.);
#4656=ORIENTED_EDGE('',*,*,#3687,.T.);
#4657=ORIENTED_EDGE('',*,*,#3688,.T.);
#4658=ORIENTED_EDGE('',*,*,#3687,.F.);
#4659=ORIENTED_EDGE('',*,*,#3686,.T.);
#4660=ORIENTED_EDGE('',*,*,#3683,.T.);
#4661=ORIENTED_EDGE('',*,*,#3688,.F.);
#4662=ORIENTED_EDGE('',*,*,#3685,.F.);
#4663=ORIENTED_EDGE('',*,*,#3689,.F.);
#4664=ORIENTED_EDGE('',*,*,#3690,.T.);
#4665=ORIENTED_EDGE('',*,*,#3691,.F.);
#4666=ORIENTED_EDGE('',*,*,#3690,.F.);
#4667=ORIENTED_EDGE('',*,*,#3692,.F.);
#4668=ORIENTED_EDGE('',*,*,#3693,.T.);
#4669=ORIENTED_EDGE('',*,*,#3694,.F.);
#4670=ORIENTED_EDGE('',*,*,#3693,.F.);
#4671=ORIENTED_EDGE('',*,*,#3695,.F.);
#4672=ORIENTED_EDGE('',*,*,#3696,.T.);
#4673=ORIENTED_EDGE('',*,*,#3697,.F.);
#4674=ORIENTED_EDGE('',*,*,#3696,.F.);
#4675=ORIENTED_EDGE('',*,*,#3698,.F.);
#4676=ORIENTED_EDGE('',*,*,#3699,.T.);
#4677=ORIENTED_EDGE('',*,*,#3700,.F.);
#4678=ORIENTED_EDGE('',*,*,#3699,.F.);
#4679=ORIENTED_EDGE('',*,*,#3701,.F.);
#4680=ORIENTED_EDGE('',*,*,#3702,.T.);
#4681=ORIENTED_EDGE('',*,*,#3703,.F.);
#4682=ORIENTED_EDGE('',*,*,#3702,.F.);
#4683=ORIENTED_EDGE('',*,*,#3701,.T.);
#4684=ORIENTED_EDGE('',*,*,#3704,.T.);
#4685=ORIENTED_EDGE('',*,*,#3704,.F.);
#4686=ORIENTED_EDGE('',*,*,#3705,.T.);
#4687=ORIENTED_EDGE('',*,*,#3706,.T.);
#4688=ORIENTED_EDGE('',*,*,#3705,.F.);
#4689=ORIENTED_EDGE('',*,*,#3707,.F.);
#4690=ORIENTED_EDGE('',*,*,#3708,.T.);
#4691=ORIENTED_EDGE('',*,*,#3709,.T.);
#4692=ORIENTED_EDGE('',*,*,#3708,.F.);
#4693=ORIENTED_EDGE('',*,*,#3707,.T.);
#4694=ORIENTED_EDGE('',*,*,#3703,.T.);
#4695=ORIENTED_EDGE('',*,*,#3700,.T.);
#4696=ORIENTED_EDGE('',*,*,#3697,.T.);
#4697=ORIENTED_EDGE('',*,*,#3694,.T.);
#4698=ORIENTED_EDGE('',*,*,#3691,.T.);
#4699=ORIENTED_EDGE('',*,*,#3709,.F.);
#4700=ORIENTED_EDGE('',*,*,#3706,.F.);
#4701=ORIENTED_EDGE('',*,*,#3698,.T.);
#4702=ORIENTED_EDGE('',*,*,#3695,.T.);
#4703=ORIENTED_EDGE('',*,*,#3692,.T.);
#4704=ORIENTED_EDGE('',*,*,#3689,.T.);
#4705=ORIENTED_EDGE('',*,*,#3710,.F.);
#4706=ORIENTED_EDGE('',*,*,#3711,.T.);
#4707=ORIENTED_EDGE('',*,*,#3712,.F.);
#4708=ORIENTED_EDGE('',*,*,#3711,.F.);
#4709=ORIENTED_EDGE('',*,*,#3713,.F.);
#4710=ORIENTED_EDGE('',*,*,#3714,.T.);
#4711=ORIENTED_EDGE('',*,*,#3715,.F.);
#4712=ORIENTED_EDGE('',*,*,#3714,.F.);
#4713=ORIENTED_EDGE('',*,*,#3716,.F.);
#4714=ORIENTED_EDGE('',*,*,#3717,.T.);
#4715=ORIENTED_EDGE('',*,*,#3718,.F.);
#4716=ORIENTED_EDGE('',*,*,#3717,.F.);
#4717=ORIENTED_EDGE('',*,*,#3719,.F.);
#4718=ORIENTED_EDGE('',*,*,#3720,.T.);
#4719=ORIENTED_EDGE('',*,*,#3721,.F.);
#4720=ORIENTED_EDGE('',*,*,#3720,.F.);
#4721=ORIENTED_EDGE('',*,*,#3722,.F.);
#4722=ORIENTED_EDGE('',*,*,#3723,.T.);
#4723=ORIENTED_EDGE('',*,*,#3724,.T.);
#4724=ORIENTED_EDGE('',*,*,#3723,.F.);
#4725=ORIENTED_EDGE('',*,*,#3724,.F.);
#4726=ORIENTED_EDGE('',*,*,#3725,.F.);
#4727=ORIENTED_EDGE('',*,*,#3726,.F.);
#4728=ORIENTED_EDGE('',*,*,#3727,.T.);
#4729=ORIENTED_EDGE('',*,*,#3725,.T.);
#4730=ORIENTED_EDGE('',*,*,#3727,.F.);
#4731=ORIENTED_EDGE('',*,*,#3728,.F.);
#4732=ORIENTED_EDGE('',*,*,#3729,.T.);
#4733=ORIENTED_EDGE('',*,*,#3730,.T.);
#4734=ORIENTED_EDGE('',*,*,#3729,.F.);
#4735=ORIENTED_EDGE('',*,*,#3728,.T.);
#4736=ORIENTED_EDGE('',*,*,#3726,.T.);
#4737=ORIENTED_EDGE('',*,*,#3721,.T.);
#4738=ORIENTED_EDGE('',*,*,#3718,.T.);
#4739=ORIENTED_EDGE('',*,*,#3715,.T.);
#4740=ORIENTED_EDGE('',*,*,#3712,.T.);
#4741=ORIENTED_EDGE('',*,*,#3730,.F.);
#4742=ORIENTED_EDGE('',*,*,#3722,.T.);
#4743=ORIENTED_EDGE('',*,*,#3719,.T.);
#4744=ORIENTED_EDGE('',*,*,#3716,.T.);
#4745=ORIENTED_EDGE('',*,*,#3713,.T.);
#4746=ORIENTED_EDGE('',*,*,#3710,.T.);
#4747=ORIENTED_EDGE('',*,*,#3731,.T.);
#4748=ORIENTED_EDGE('',*,*,#3732,.T.);
#4749=ORIENTED_EDGE('',*,*,#3733,.F.);
#4750=ORIENTED_EDGE('',*,*,#3734,.F.);
#4751=ORIENTED_EDGE('',*,*,#3735,.T.);
#4752=ORIENTED_EDGE('',*,*,#3734,.T.);
#4753=ORIENTED_EDGE('',*,*,#3736,.F.);
#4754=ORIENTED_EDGE('',*,*,#3737,.F.);
#4755=ORIENTED_EDGE('',*,*,#3738,.T.);
#4756=ORIENTED_EDGE('',*,*,#3737,.T.);
#4757=ORIENTED_EDGE('',*,*,#3739,.F.);
#4758=ORIENTED_EDGE('',*,*,#3740,.F.);
#4759=ORIENTED_EDGE('',*,*,#3741,.T.);
#4760=ORIENTED_EDGE('',*,*,#3740,.T.);
#4761=ORIENTED_EDGE('',*,*,#3742,.F.);
#4762=ORIENTED_EDGE('',*,*,#3732,.F.);
#4763=ORIENTED_EDGE('',*,*,#3742,.T.);
#4764=ORIENTED_EDGE('',*,*,#3739,.T.);
#4765=ORIENTED_EDGE('',*,*,#3736,.T.);
#4766=ORIENTED_EDGE('',*,*,#3733,.T.);
#4767=ORIENTED_EDGE('',*,*,#3741,.F.);
#4768=ORIENTED_EDGE('',*,*,#3731,.F.);
#4769=ORIENTED_EDGE('',*,*,#3735,.F.);
#4770=ORIENTED_EDGE('',*,*,#3738,.F.);
#4771=ORIENTED_EDGE('',*,*,#3743,.T.);
#4772=ORIENTED_EDGE('',*,*,#3744,.T.);
#4773=ORIENTED_EDGE('',*,*,#3745,.F.);
#4774=ORIENTED_EDGE('',*,*,#3746,.F.);
#4775=ORIENTED_EDGE('',*,*,#3747,.T.);
#4776=ORIENTED_EDGE('',*,*,#3746,.T.);
#4777=ORIENTED_EDGE('',*,*,#3748,.F.);
#4778=ORIENTED_EDGE('',*,*,#3749,.F.);
#4779=ORIENTED_EDGE('',*,*,#3750,.T.);
#4780=ORIENTED_EDGE('',*,*,#3749,.T.);
#4781=ORIENTED_EDGE('',*,*,#3751,.F.);
#4782=ORIENTED_EDGE('',*,*,#3752,.F.);
#4783=ORIENTED_EDGE('',*,*,#3753,.T.);
#4784=ORIENTED_EDGE('',*,*,#3752,.T.);
#4785=ORIENTED_EDGE('',*,*,#3754,.F.);
#4786=ORIENTED_EDGE('',*,*,#3744,.F.);
#4787=ORIENTED_EDGE('',*,*,#3754,.T.);
#4788=ORIENTED_EDGE('',*,*,#3751,.T.);
#4789=ORIENTED_EDGE('',*,*,#3748,.T.);
#4790=ORIENTED_EDGE('',*,*,#3745,.T.);
#4791=ORIENTED_EDGE('',*,*,#3753,.F.);
#4792=ORIENTED_EDGE('',*,*,#3743,.F.);
#4793=ORIENTED_EDGE('',*,*,#3747,.F.);
#4794=ORIENTED_EDGE('',*,*,#3750,.F.);
#4795=ORIENTED_EDGE('',*,*,#3755,.F.);
#4796=ORIENTED_EDGE('',*,*,#3756,.F.);
#4797=ORIENTED_EDGE('',*,*,#3757,.T.);
#4798=ORIENTED_EDGE('',*,*,#3758,.F.);
#4799=ORIENTED_EDGE('',*,*,#3759,.F.);
#4800=ORIENTED_EDGE('',*,*,#3757,.F.);
#4801=ORIENTED_EDGE('',*,*,#3758,.T.);
#4802=ORIENTED_EDGE('',*,*,#3759,.T.);
#4803=ORIENTED_EDGE('',*,*,#3760,.T.);
#4804=ORIENTED_EDGE('',*,*,#3761,.T.);
#4805=ORIENTED_EDGE('',*,*,#3760,.F.);
#4806=ORIENTED_EDGE('',*,*,#3762,.T.);
#4807=ORIENTED_EDGE('',*,*,#3763,.T.);
#4808=ORIENTED_EDGE('',*,*,#3764,.F.);
#4809=ORIENTED_EDGE('',*,*,#3763,.F.);
#4810=ORIENTED_EDGE('',*,*,#3764,.T.);
#4811=ORIENTED_EDGE('',*,*,#3765,.T.);
#4812=ORIENTED_EDGE('',*,*,#3766,.F.);
#4813=ORIENTED_EDGE('',*,*,#3765,.F.);
#4814=ORIENTED_EDGE('',*,*,#3761,.F.);
#4815=ORIENTED_EDGE('',*,*,#3766,.T.);
#4816=ORIENTED_EDGE('',*,*,#3767,.F.);
#4817=ORIENTED_EDGE('',*,*,#3768,.T.);
#4818=ORIENTED_EDGE('',*,*,#3755,.T.);
#4819=ORIENTED_EDGE('',*,*,#3756,.T.);
#4820=ORIENTED_EDGE('',*,*,#3768,.F.);
#4821=ORIENTED_EDGE('',*,*,#3767,.T.);
#4822=ORIENTED_EDGE('',*,*,#3769,.F.);
#4823=ORIENTED_EDGE('',*,*,#3769,.T.);
#4824=ORIENTED_EDGE('',*,*,#3770,.T.);
#4825=ORIENTED_EDGE('',*,*,#3762,.F.);
#4826=ORIENTED_EDGE('',*,*,#3770,.F.);
#4827=ORIENTED_EDGE('',*,*,#3771,.F.);
#4828=ORIENTED_EDGE('',*,*,#3772,.F.);
#4829=ORIENTED_EDGE('',*,*,#3773,.T.);
#4830=ORIENTED_EDGE('',*,*,#3774,.F.);
#4831=ORIENTED_EDGE('',*,*,#3775,.F.);
#4832=ORIENTED_EDGE('',*,*,#3773,.F.);
#4833=ORIENTED_EDGE('',*,*,#3776,.T.);
#4834=ORIENTED_EDGE('',*,*,#3777,.T.);
#4835=ORIENTED_EDGE('',*,*,#3774,.T.);
#4836=ORIENTED_EDGE('',*,*,#3775,.T.);
#4837=ORIENTED_EDGE('',*,*,#3777,.F.);
#4838=ORIENTED_EDGE('',*,*,#3778,.F.);
#4839=ORIENTED_EDGE('',*,*,#3779,.T.);
#4840=ORIENTED_EDGE('',*,*,#3780,.F.);
#4841=ORIENTED_EDGE('',*,*,#3781,.T.);
#4842=ORIENTED_EDGE('',*,*,#3778,.T.);
#4843=ORIENTED_EDGE('',*,*,#3781,.F.);
#4844=ORIENTED_EDGE('',*,*,#3782,.F.);
#4845=ORIENTED_EDGE('',*,*,#3783,.T.);
#4846=ORIENTED_EDGE('',*,*,#3780,.T.);
#4847=ORIENTED_EDGE('',*,*,#3783,.F.);
#4848=ORIENTED_EDGE('',*,*,#3784,.F.);
#4849=ORIENTED_EDGE('',*,*,#3785,.T.);
#4850=ORIENTED_EDGE('',*,*,#3782,.T.);
#4851=ORIENTED_EDGE('',*,*,#3785,.F.);
#4852=ORIENTED_EDGE('',*,*,#3784,.T.);
#4853=ORIENTED_EDGE('',*,*,#3776,.F.);
#4854=ORIENTED_EDGE('',*,*,#3771,.T.);
#4855=ORIENTED_EDGE('',*,*,#3772,.T.);
#4856=ORIENTED_EDGE('',*,*,#3786,.T.);
#4857=ORIENTED_EDGE('',*,*,#3779,.F.);
#4858=ORIENTED_EDGE('',*,*,#3786,.F.);
#4859=ORIENTED_EDGE('',*,*,#3787,.T.);
#4860=ORIENTED_EDGE('',*,*,#3787,.F.);
#4861=ORIENTED_EDGE('',*,*,#3788,.T.);
#4862=ORIENTED_EDGE('',*,*,#3788,.F.);
#4863=ORIENTED_EDGE('',*,*,#3789,.T.);
#4864=ORIENTED_EDGE('',*,*,#3789,.F.);
#4865=ORIENTED_EDGE('',*,*,#3790,.T.);
#4866=ORIENTED_EDGE('',*,*,#3790,.F.);
#4867=ORIENTED_EDGE('',*,*,#3791,.T.);
#4868=ORIENTED_EDGE('',*,*,#3791,.F.);
#4869=ORIENTED_EDGE('',*,*,#3792,.T.);
#4870=ORIENTED_EDGE('',*,*,#3792,.F.);
#4871=ORIENTED_EDGE('',*,*,#3793,.T.);
#4872=ORIENTED_EDGE('',*,*,#3793,.F.);
#4873=ORIENTED_EDGE('',*,*,#3794,.T.);
#4874=ORIENTED_EDGE('',*,*,#3794,.F.);
#4875=ORIENTED_EDGE('',*,*,#3795,.T.);
#4876=ORIENTED_EDGE('',*,*,#3795,.F.);
#4877=ORIENTED_EDGE('',*,*,#3796,.F.);
#4878=ORIENTED_EDGE('',*,*,#3797,.F.);
#4879=ORIENTED_EDGE('',*,*,#3798,.F.);
#4880=ORIENTED_EDGE('',*,*,#3799,.F.);
#4881=ORIENTED_EDGE('',*,*,#3798,.T.);
#4882=ORIENTED_EDGE('',*,*,#3800,.F.);
#4883=ORIENTED_EDGE('',*,*,#3801,.T.);
#4884=ORIENTED_EDGE('',*,*,#3802,.F.);
#4885=ORIENTED_EDGE('',*,*,#3803,.T.);
#4886=ORIENTED_EDGE('',*,*,#3804,.F.);
#4887=ORIENTED_EDGE('',*,*,#3805,.T.);
#4888=ORIENTED_EDGE('',*,*,#3806,.F.);
#4889=ORIENTED_EDGE('',*,*,#3807,.T.);
#4890=ORIENTED_EDGE('',*,*,#3808,.F.);
#4891=ORIENTED_EDGE('',*,*,#3807,.F.);
#4892=ORIENTED_EDGE('',*,*,#3809,.F.);
#4893=ORIENTED_EDGE('',*,*,#3810,.T.);
#4894=ORIENTED_EDGE('',*,*,#3811,.F.);
#4895=ORIENTED_EDGE('',*,*,#3812,.T.);
#4896=ORIENTED_EDGE('',*,*,#3813,.F.);
#4897=ORIENTED_EDGE('',*,*,#3814,.T.);
#4898=ORIENTED_EDGE('',*,*,#3815,.F.);
#4899=ORIENTED_EDGE('',*,*,#3816,.T.);
#4900=ORIENTED_EDGE('',*,*,#3817,.F.);
#4901=ORIENTED_EDGE('',*,*,#3818,.T.);
#4902=ORIENTED_EDGE('',*,*,#3819,.F.);
#4903=ORIENTED_EDGE('',*,*,#3797,.T.);
#4904=ORIENTED_EDGE('',*,*,#3820,.T.);
#4905=ORIENTED_EDGE('',*,*,#3821,.T.);
#4906=ORIENTED_EDGE('',*,*,#3800,.T.);
#4907=ORIENTED_EDGE('',*,*,#3822,.F.);
#4908=ORIENTED_EDGE('',*,*,#3823,.F.);
#4909=ORIENTED_EDGE('',*,*,#3801,.F.);
#4910=ORIENTED_EDGE('',*,*,#3821,.F.);
#4911=ORIENTED_EDGE('',*,*,#3823,.T.);
#4912=ORIENTED_EDGE('',*,*,#3824,.T.);
#4913=ORIENTED_EDGE('',*,*,#3825,.T.);
#4914=ORIENTED_EDGE('',*,*,#3802,.T.);
#4915=ORIENTED_EDGE('',*,*,#3826,.F.);
#4916=ORIENTED_EDGE('',*,*,#3827,.F.);
#4917=ORIENTED_EDGE('',*,*,#3803,.F.);
#4918=ORIENTED_EDGE('',*,*,#3825,.F.);
#4919=ORIENTED_EDGE('',*,*,#3827,.T.);
#4920=ORIENTED_EDGE('',*,*,#3828,.T.);
#4921=ORIENTED_EDGE('',*,*,#3829,.T.);
#4922=ORIENTED_EDGE('',*,*,#3804,.T.);
#4923=ORIENTED_EDGE('',*,*,#3830,.F.);
#4924=ORIENTED_EDGE('',*,*,#3831,.F.);
#4925=ORIENTED_EDGE('',*,*,#3805,.F.);
#4926=ORIENTED_EDGE('',*,*,#3829,.F.);
#4927=ORIENTED_EDGE('',*,*,#3831,.T.);
#4928=ORIENTED_EDGE('',*,*,#3832,.T.);
#4929=ORIENTED_EDGE('',*,*,#3833,.T.);
#4930=ORIENTED_EDGE('',*,*,#3834,.T.);
#4931=ORIENTED_EDGE('',*,*,#3809,.T.);
#4932=ORIENTED_EDGE('',*,*,#3806,.T.);
#4933=ORIENTED_EDGE('',*,*,#3835,.F.);
#4934=ORIENTED_EDGE('',*,*,#3836,.F.);
#4935=ORIENTED_EDGE('',*,*,#3810,.F.);
#4936=ORIENTED_EDGE('',*,*,#3834,.F.);
#4937=ORIENTED_EDGE('',*,*,#3836,.T.);
#4938=ORIENTED_EDGE('',*,*,#3837,.T.);
#4939=ORIENTED_EDGE('',*,*,#3838,.T.);
#4940=ORIENTED_EDGE('',*,*,#3811,.T.);
#4941=ORIENTED_EDGE('',*,*,#3839,.F.);
#4942=ORIENTED_EDGE('',*,*,#3840,.F.);
#4943=ORIENTED_EDGE('',*,*,#3812,.F.);
#4944=ORIENTED_EDGE('',*,*,#3838,.F.);
#4945=ORIENTED_EDGE('',*,*,#3840,.T.);
#4946=ORIENTED_EDGE('',*,*,#3841,.T.);
#4947=ORIENTED_EDGE('',*,*,#3842,.T.);
#4948=ORIENTED_EDGE('',*,*,#3813,.T.);
#4949=ORIENTED_EDGE('',*,*,#3843,.F.);
#4950=ORIENTED_EDGE('',*,*,#3844,.F.);
#4951=ORIENTED_EDGE('',*,*,#3814,.F.);
#4952=ORIENTED_EDGE('',*,*,#3842,.F.);
#4953=ORIENTED_EDGE('',*,*,#3844,.T.);
#4954=ORIENTED_EDGE('',*,*,#3845,.T.);
#4955=ORIENTED_EDGE('',*,*,#3846,.T.);
#4956=ORIENTED_EDGE('',*,*,#3815,.T.);
#4957=ORIENTED_EDGE('',*,*,#3816,.F.);
#4958=ORIENTED_EDGE('',*,*,#3846,.F.);
#4959=ORIENTED_EDGE('',*,*,#3847,.F.);
#4960=ORIENTED_EDGE('',*,*,#3848,.F.);
#4961=ORIENTED_EDGE('',*,*,#3849,.F.);
#4962=ORIENTED_EDGE('',*,*,#3850,.T.);
#4963=ORIENTED_EDGE('',*,*,#3832,.F.);
#4964=ORIENTED_EDGE('',*,*,#3830,.T.);
#4965=ORIENTED_EDGE('',*,*,#3828,.F.);
#4966=ORIENTED_EDGE('',*,*,#3826,.T.);
#4967=ORIENTED_EDGE('',*,*,#3824,.F.);
#4968=ORIENTED_EDGE('',*,*,#3822,.T.);
#4969=ORIENTED_EDGE('',*,*,#3820,.F.);
#4970=ORIENTED_EDGE('',*,*,#3796,.T.);
#4971=ORIENTED_EDGE('',*,*,#3851,.F.);
#4972=ORIENTED_EDGE('',*,*,#3852,.T.);
#4973=ORIENTED_EDGE('',*,*,#3853,.F.);
#4974=ORIENTED_EDGE('',*,*,#3847,.T.);
#4975=ORIENTED_EDGE('',*,*,#3845,.F.);
#4976=ORIENTED_EDGE('',*,*,#3843,.T.);
#4977=ORIENTED_EDGE('',*,*,#3841,.F.);
#4978=ORIENTED_EDGE('',*,*,#3839,.T.);
#4979=ORIENTED_EDGE('',*,*,#3837,.F.);
#4980=ORIENTED_EDGE('',*,*,#3835,.T.);
#4981=ORIENTED_EDGE('',*,*,#3833,.F.);
#4982=ORIENTED_EDGE('',*,*,#3850,.F.);
#4983=ORIENTED_EDGE('',*,*,#3799,.T.);
#4984=ORIENTED_EDGE('',*,*,#3819,.T.);
#4985=ORIENTED_EDGE('',*,*,#3854,.T.);
#4986=ORIENTED_EDGE('',*,*,#3851,.T.);
#4987=ORIENTED_EDGE('',*,*,#3818,.F.);
#4988=ORIENTED_EDGE('',*,*,#3855,.F.);
#4989=ORIENTED_EDGE('',*,*,#3852,.F.);
#4990=ORIENTED_EDGE('',*,*,#3854,.F.);
#4991=ORIENTED_EDGE('',*,*,#3808,.T.);
#4992=ORIENTED_EDGE('',*,*,#3849,.T.);
#4993=ORIENTED_EDGE('',*,*,#3848,.T.);
#4994=ORIENTED_EDGE('',*,*,#3853,.T.);
#4995=ORIENTED_EDGE('',*,*,#3855,.T.);
#4996=ORIENTED_EDGE('',*,*,#3817,.T.);
#4997=ORIENTED_EDGE('',*,*,#3856,.F.);
#4998=ORIENTED_EDGE('',*,*,#3857,.T.);
#4999=ORIENTED_EDGE('',*,*,#3858,.F.);
#5000=ORIENTED_EDGE('',*,*,#3859,.T.);
#5001=ORIENTED_EDGE('',*,*,#3856,.T.);
#5002=ORIENTED_EDGE('',*,*,#3859,.F.);
#5003=ORIENTED_EDGE('',*,*,#3858,.T.);
#5004=ORIENTED_EDGE('',*,*,#3860,.F.);
#5005=ORIENTED_EDGE('',*,*,#3860,.T.);
#5006=ORIENTED_EDGE('',*,*,#3861,.T.);
#5007=ORIENTED_EDGE('',*,*,#3857,.F.);
#5008=ORIENTED_EDGE('',*,*,#3861,.F.);
#5009=ORIENTED_EDGE('',*,*,#3862,.F.);
#5010=ORIENTED_EDGE('',*,*,#3863,.T.);
#5011=ORIENTED_EDGE('',*,*,#3864,.F.);
#5012=ORIENTED_EDGE('',*,*,#3865,.T.);
#5013=ORIENTED_EDGE('',*,*,#3862,.T.);
#5014=ORIENTED_EDGE('',*,*,#3865,.F.);
#5015=ORIENTED_EDGE('',*,*,#3864,.T.);
#5016=ORIENTED_EDGE('',*,*,#3866,.F.);
#5017=ORIENTED_EDGE('',*,*,#3866,.T.);
#5018=ORIENTED_EDGE('',*,*,#3867,.T.);
#5019=ORIENTED_EDGE('',*,*,#3863,.F.);
#5020=ORIENTED_EDGE('',*,*,#3867,.F.);
#5021=ORIENTED_EDGE('',*,*,#3868,.F.);
#5022=ORIENTED_EDGE('',*,*,#3869,.F.);
#5023=ORIENTED_EDGE('',*,*,#3870,.T.);
#5024=ORIENTED_EDGE('',*,*,#3868,.T.);
#5025=ORIENTED_EDGE('',*,*,#3870,.F.);
#5026=ORIENTED_EDGE('',*,*,#3871,.F.);
#5027=ORIENTED_EDGE('',*,*,#3872,.T.);
#5028=ORIENTED_EDGE('',*,*,#3869,.T.);
#5029=ORIENTED_EDGE('',*,*,#3872,.F.);
#5030=ORIENTED_EDGE('',*,*,#3873,.F.);
#5031=ORIENTED_EDGE('',*,*,#3874,.T.);
#5032=ORIENTED_EDGE('',*,*,#3871,.T.);
#5033=ORIENTED_EDGE('',*,*,#3874,.F.);
#5034=ORIENTED_EDGE('',*,*,#3873,.T.);
#5035=ORIENTED_EDGE('',*,*,#3875,.F.);
#5036=ORIENTED_EDGE('',*,*,#3876,.F.);
#5037=ORIENTED_EDGE('',*,*,#3877,.T.);
#5038=ORIENTED_EDGE('',*,*,#3875,.T.);
#5039=ORIENTED_EDGE('',*,*,#3877,.F.);
#5040=ORIENTED_EDGE('',*,*,#3878,.F.);
#5041=ORIENTED_EDGE('',*,*,#3879,.T.);
#5042=ORIENTED_EDGE('',*,*,#3876,.T.);
#5043=ORIENTED_EDGE('',*,*,#3879,.F.);
#5044=ORIENTED_EDGE('',*,*,#3880,.F.);
#5045=ORIENTED_EDGE('',*,*,#3881,.T.);
#5046=ORIENTED_EDGE('',*,*,#3878,.T.);
#5047=ORIENTED_EDGE('',*,*,#3881,.F.);
#5048=ORIENTED_EDGE('',*,*,#3880,.T.);
#5049=ORIENTED_EDGE('',*,*,#3882,.T.);
#5050=ORIENTED_EDGE('',*,*,#3883,.T.);
#5051=ORIENTED_EDGE('',*,*,#3884,.T.);
#5052=ORIENTED_EDGE('',*,*,#3885,.F.);
#5053=ORIENTED_EDGE('',*,*,#3886,.T.);
#5054=ORIENTED_EDGE('',*,*,#3887,.T.);
#5055=ORIENTED_EDGE('',*,*,#3888,.T.);
#5056=ORIENTED_EDGE('',*,*,#3883,.F.);
#5057=ORIENTED_EDGE('',*,*,#3889,.T.);
#5058=ORIENTED_EDGE('',*,*,#3890,.T.);
#5059=ORIENTED_EDGE('',*,*,#3891,.T.);
#5060=ORIENTED_EDGE('',*,*,#3887,.F.);
#5061=ORIENTED_EDGE('',*,*,#3892,.T.);
#5062=ORIENTED_EDGE('',*,*,#3893,.T.);
#5063=ORIENTED_EDGE('',*,*,#3894,.T.);
#5064=ORIENTED_EDGE('',*,*,#3890,.F.);
#5065=ORIENTED_EDGE('',*,*,#3895,.T.);
#5066=ORIENTED_EDGE('',*,*,#3896,.T.);
#5067=ORIENTED_EDGE('',*,*,#3897,.T.);
#5068=ORIENTED_EDGE('',*,*,#3893,.F.);
#5069=ORIENTED_EDGE('',*,*,#3898,.T.);
#5070=ORIENTED_EDGE('',*,*,#3885,.T.);
#5071=ORIENTED_EDGE('',*,*,#3899,.T.);
#5072=ORIENTED_EDGE('',*,*,#3896,.F.);
#5073=ORIENTED_EDGE('',*,*,#3898,.F.);
#5074=ORIENTED_EDGE('',*,*,#3895,.F.);
#5075=ORIENTED_EDGE('',*,*,#3892,.F.);
#5076=ORIENTED_EDGE('',*,*,#3889,.F.);
#5077=ORIENTED_EDGE('',*,*,#3886,.F.);
#5078=ORIENTED_EDGE('',*,*,#3882,.F.);
#5079=ORIENTED_EDGE('',*,*,#3899,.F.);
#5080=ORIENTED_EDGE('',*,*,#3884,.F.);
#5081=ORIENTED_EDGE('',*,*,#3888,.F.);
#5082=ORIENTED_EDGE('',*,*,#3891,.F.);
#5083=ORIENTED_EDGE('',*,*,#3894,.F.);
#5084=ORIENTED_EDGE('',*,*,#3897,.F.);
#5085=ORIENTED_EDGE('',*,*,#3900,.F.);
#5086=ORIENTED_EDGE('',*,*,#3901,.F.);
#5087=ORIENTED_EDGE('',*,*,#3902,.T.);
#5088=ORIENTED_EDGE('',*,*,#3900,.T.);
#5089=ORIENTED_EDGE('',*,*,#3902,.F.);
#5090=ORIENTED_EDGE('',*,*,#3903,.F.);
#5091=ORIENTED_EDGE('',*,*,#3904,.T.);
#5092=ORIENTED_EDGE('',*,*,#3901,.T.);
#5093=ORIENTED_EDGE('',*,*,#3904,.F.);
#5094=ORIENTED_EDGE('',*,*,#3905,.F.);
#5095=ORIENTED_EDGE('',*,*,#3906,.T.);
#5096=ORIENTED_EDGE('',*,*,#3903,.T.);
#5097=ORIENTED_EDGE('',*,*,#3906,.F.);
#5098=ORIENTED_EDGE('',*,*,#3905,.T.);
#5099=ORIENTED_EDGE('',*,*,#3907,.F.);
#5100=ORIENTED_EDGE('',*,*,#3908,.F.);
#5101=ORIENTED_EDGE('',*,*,#3909,.T.);
#5102=ORIENTED_EDGE('',*,*,#3907,.T.);
#5103=ORIENTED_EDGE('',*,*,#3909,.F.);
#5104=ORIENTED_EDGE('',*,*,#3910,.F.);
#5105=ORIENTED_EDGE('',*,*,#3911,.T.);
#5106=ORIENTED_EDGE('',*,*,#3908,.T.);
#5107=ORIENTED_EDGE('',*,*,#3911,.F.);
#5108=ORIENTED_EDGE('',*,*,#3912,.F.);
#5109=ORIENTED_EDGE('',*,*,#3913,.T.);
#5110=ORIENTED_EDGE('',*,*,#3910,.T.);
#5111=ORIENTED_EDGE('',*,*,#3913,.F.);
#5112=ORIENTED_EDGE('',*,*,#3912,.T.);
#5113=ORIENTED_EDGE('',*,*,#3914,.T.);
#5114=ORIENTED_EDGE('',*,*,#3915,.T.);
#5115=ORIENTED_EDGE('',*,*,#3916,.T.);
#5116=ORIENTED_EDGE('',*,*,#3917,.F.);
#5117=ORIENTED_EDGE('',*,*,#3918,.T.);
#5118=ORIENTED_EDGE('',*,*,#3919,.T.);
#5119=ORIENTED_EDGE('',*,*,#3920,.T.);
#5120=ORIENTED_EDGE('',*,*,#3915,.F.);
#5121=ORIENTED_EDGE('',*,*,#3921,.T.);
#5122=ORIENTED_EDGE('',*,*,#3922,.T.);
#5123=ORIENTED_EDGE('',*,*,#3923,.T.);
#5124=ORIENTED_EDGE('',*,*,#3919,.F.);
#5125=ORIENTED_EDGE('',*,*,#3924,.T.);
#5126=ORIENTED_EDGE('',*,*,#3925,.T.);
#5127=ORIENTED_EDGE('',*,*,#3926,.T.);
#5128=ORIENTED_EDGE('',*,*,#3922,.F.);
#5129=ORIENTED_EDGE('',*,*,#3927,.T.);
#5130=ORIENTED_EDGE('',*,*,#3928,.T.);
#5131=ORIENTED_EDGE('',*,*,#3929,.T.);
#5132=ORIENTED_EDGE('',*,*,#3925,.F.);
#5133=ORIENTED_EDGE('',*,*,#3930,.T.);
#5134=ORIENTED_EDGE('',*,*,#3917,.T.);
#5135=ORIENTED_EDGE('',*,*,#3931,.T.);
#5136=ORIENTED_EDGE('',*,*,#3928,.F.);
#5137=ORIENTED_EDGE('',*,*,#3930,.F.);
#5138=ORIENTED_EDGE('',*,*,#3927,.F.);
#5139=ORIENTED_EDGE('',*,*,#3924,.F.);
#5140=ORIENTED_EDGE('',*,*,#3921,.F.);
#5141=ORIENTED_EDGE('',*,*,#3918,.F.);
#5142=ORIENTED_EDGE('',*,*,#3914,.F.);
#5143=ORIENTED_EDGE('',*,*,#3931,.F.);
#5144=ORIENTED_EDGE('',*,*,#3916,.F.);
#5145=ORIENTED_EDGE('',*,*,#3920,.F.);
#5146=ORIENTED_EDGE('',*,*,#3923,.F.);
#5147=ORIENTED_EDGE('',*,*,#3926,.F.);
#5148=ORIENTED_EDGE('',*,*,#3929,.F.);
#5149=ORIENTED_EDGE('',*,*,#3932,.F.);
#5150=ORIENTED_EDGE('',*,*,#3933,.T.);
#5151=ORIENTED_EDGE('',*,*,#3934,.F.);
#5152=ORIENTED_EDGE('',*,*,#3935,.T.);
#5153=ORIENTED_EDGE('',*,*,#3936,.F.);
#5154=ORIENTED_EDGE('',*,*,#3935,.F.);
#5155=ORIENTED_EDGE('',*,*,#3937,.F.);
#5156=ORIENTED_EDGE('',*,*,#3938,.F.);
#5157=ORIENTED_EDGE('',*,*,#3939,.F.);
#5158=ORIENTED_EDGE('',*,*,#3938,.T.);
#5159=ORIENTED_EDGE('',*,*,#3940,.T.);
#5160=ORIENTED_EDGE('',*,*,#3941,.T.);
#5161=ORIENTED_EDGE('',*,*,#3937,.T.);
#5162=ORIENTED_EDGE('',*,*,#3934,.T.);
#5163=ORIENTED_EDGE('',*,*,#3942,.T.);
#5164=ORIENTED_EDGE('',*,*,#3940,.F.);
#5165=ORIENTED_EDGE('',*,*,#3943,.F.);
#5166=ORIENTED_EDGE('',*,*,#3941,.F.);
#5167=ORIENTED_EDGE('',*,*,#3942,.F.);
#5168=ORIENTED_EDGE('',*,*,#3933,.F.);
#5169=ORIENTED_EDGE('',*,*,#3944,.F.);
#5170=ORIENTED_EDGE('',*,*,#3945,.T.);
#5171=ORIENTED_EDGE('',*,*,#3946,.F.);
#5172=ORIENTED_EDGE('',*,*,#3947,.T.);
#5173=ORIENTED_EDGE('',*,*,#3948,.F.);
#5174=ORIENTED_EDGE('',*,*,#3947,.F.);
#5175=ORIENTED_EDGE('',*,*,#3949,.F.);
#5176=ORIENTED_EDGE('',*,*,#3950,.F.);
#5177=ORIENTED_EDGE('',*,*,#3951,.F.);
#5178=ORIENTED_EDGE('',*,*,#3950,.T.);
#5179=ORIENTED_EDGE('',*,*,#3952,.T.);
#5180=ORIENTED_EDGE('',*,*,#3953,.T.);
#5181=ORIENTED_EDGE('',*,*,#3949,.T.);
#5182=ORIENTED_EDGE('',*,*,#3946,.T.);
#5183=ORIENTED_EDGE('',*,*,#3954,.T.);
#5184=ORIENTED_EDGE('',*,*,#3952,.F.);
#5185=ORIENTED_EDGE('',*,*,#3955,.F.);
#5186=ORIENTED_EDGE('',*,*,#3953,.F.);
#5187=ORIENTED_EDGE('',*,*,#3954,.F.);
#5188=ORIENTED_EDGE('',*,*,#3945,.F.);
#5189=ORIENTED_EDGE('',*,*,#3956,.T.);
#5190=ORIENTED_EDGE('',*,*,#3957,.F.);
#5191=ORIENTED_EDGE('',*,*,#3958,.F.);
#5192=ORIENTED_EDGE('',*,*,#3959,.F.);
#5193=ORIENTED_EDGE('',*,*,#3956,.F.);
#5194=ORIENTED_EDGE('',*,*,#3960,.T.);
#5195=ORIENTED_EDGE('',*,*,#3958,.T.);
#5196=ORIENTED_EDGE('',*,*,#3960,.F.);
#5197=ORIENTED_EDGE('',*,*,#3959,.T.);
#5198=ORIENTED_EDGE('',*,*,#3961,.T.);
#5199=ORIENTED_EDGE('',*,*,#3962,.T.);
#5200=ORIENTED_EDGE('',*,*,#3961,.F.);
#5201=ORIENTED_EDGE('',*,*,#3951,.T.);
#5202=ORIENTED_EDGE('',*,*,#3955,.T.);
#5203=ORIENTED_EDGE('',*,*,#3944,.T.);
#5204=ORIENTED_EDGE('',*,*,#3948,.T.);
#5205=ORIENTED_EDGE('',*,*,#3963,.F.);
#5206=ORIENTED_EDGE('',*,*,#3964,.T.);
#5207=ORIENTED_EDGE('',*,*,#3957,.T.);
#5208=ORIENTED_EDGE('',*,*,#3964,.F.);
#5209=ORIENTED_EDGE('',*,*,#3939,.T.);
#5210=ORIENTED_EDGE('',*,*,#3943,.T.);
#5211=ORIENTED_EDGE('',*,*,#3932,.T.);
#5212=ORIENTED_EDGE('',*,*,#3936,.T.);
#5213=ORIENTED_EDGE('',*,*,#3963,.T.);
#5214=ORIENTED_EDGE('',*,*,#3962,.F.);
#5215=ORIENTED_EDGE('',*,*,#3965,.F.);
#5216=ORIENTED_EDGE('',*,*,#3966,.T.);
#5217=ORIENTED_EDGE('',*,*,#3967,.T.);
#5218=ORIENTED_EDGE('',*,*,#3966,.F.);
#5219=ORIENTED_EDGE('',*,*,#3968,.F.);
#5220=ORIENTED_EDGE('',*,*,#3969,.T.);
#5221=ORIENTED_EDGE('',*,*,#3970,.T.);
#5222=ORIENTED_EDGE('',*,*,#3969,.F.);
#5223=ORIENTED_EDGE('',*,*,#3968,.T.);
#5224=ORIENTED_EDGE('',*,*,#3965,.T.);
#5225=ORIENTED_EDGE('',*,*,#3970,.F.);
#5226=ORIENTED_EDGE('',*,*,#3967,.F.);
#5227=ORIENTED_EDGE('',*,*,#3971,.F.);
#5228=ORIENTED_EDGE('',*,*,#3972,.T.);
#5229=ORIENTED_EDGE('',*,*,#3973,.F.);
#5230=ORIENTED_EDGE('',*,*,#3974,.F.);
#5231=ORIENTED_EDGE('',*,*,#3975,.T.);
#5232=ORIENTED_EDGE('',*,*,#3976,.F.);
#5233=ORIENTED_EDGE('',*,*,#3977,.F.);
#5234=ORIENTED_EDGE('',*,*,#3975,.F.);
#5235=ORIENTED_EDGE('',*,*,#3978,.F.);
#5236=ORIENTED_EDGE('',*,*,#3979,.F.);
#5237=ORIENTED_EDGE('',*,*,#3972,.F.);
#5238=ORIENTED_EDGE('',*,*,#3980,.F.);
#5239=ORIENTED_EDGE('',*,*,#3978,.T.);
#5240=ORIENTED_EDGE('',*,*,#3974,.T.);
#5241=ORIENTED_EDGE('',*,*,#3981,.F.);
#5242=ORIENTED_EDGE('',*,*,#3982,.T.);
#5243=ORIENTED_EDGE('',*,*,#3983,.T.);
#5244=ORIENTED_EDGE('',*,*,#3982,.F.);
#5245=ORIENTED_EDGE('',*,*,#3979,.T.);
#5246=ORIENTED_EDGE('',*,*,#3980,.T.);
#5247=ORIENTED_EDGE('',*,*,#3973,.T.);
#5248=ORIENTED_EDGE('',*,*,#3971,.T.);
#5249=ORIENTED_EDGE('',*,*,#3984,.F.);
#5250=ORIENTED_EDGE('',*,*,#3985,.T.);
#5251=ORIENTED_EDGE('',*,*,#3986,.T.);
#5252=ORIENTED_EDGE('',*,*,#3985,.F.);
#5253=ORIENTED_EDGE('',*,*,#3976,.T.);
#5254=ORIENTED_EDGE('',*,*,#3977,.T.);
#5255=ORIENTED_EDGE('',*,*,#3984,.T.);
#5256=ORIENTED_EDGE('',*,*,#3981,.T.);
#5257=ORIENTED_EDGE('',*,*,#3986,.F.);
#5258=ORIENTED_EDGE('',*,*,#3983,.F.);
#5259=ORIENTED_EDGE('',*,*,#3987,.F.);
#5260=ORIENTED_EDGE('',*,*,#3988,.T.);
#5261=ORIENTED_EDGE('',*,*,#3989,.F.);
#5262=ORIENTED_EDGE('',*,*,#3990,.F.);
#5263=ORIENTED_EDGE('',*,*,#3991,.T.);
#5264=ORIENTED_EDGE('',*,*,#3992,.F.);
#5265=ORIENTED_EDGE('',*,*,#3993,.F.);
#5266=ORIENTED_EDGE('',*,*,#3991,.F.);
#5267=ORIENTED_EDGE('',*,*,#3994,.F.);
#5268=ORIENTED_EDGE('',*,*,#3995,.F.);
#5269=ORIENTED_EDGE('',*,*,#3988,.F.);
#5270=ORIENTED_EDGE('',*,*,#3996,.F.);
#5271=ORIENTED_EDGE('',*,*,#3994,.T.);
#5272=ORIENTED_EDGE('',*,*,#3990,.T.);
#5273=ORIENTED_EDGE('',*,*,#3997,.F.);
#5274=ORIENTED_EDGE('',*,*,#3998,.F.);
#5275=ORIENTED_EDGE('',*,*,#3999,.T.);
#5276=ORIENTED_EDGE('',*,*,#4000,.T.);
#5277=ORIENTED_EDGE('',*,*,#4001,.F.);
#5278=ORIENTED_EDGE('',*,*,#4000,.F.);
#5279=ORIENTED_EDGE('',*,*,#4002,.T.);
#5280=ORIENTED_EDGE('',*,*,#4003,.T.);
#5281=ORIENTED_EDGE('',*,*,#4004,.F.);
#5282=ORIENTED_EDGE('',*,*,#4005,.F.);
#5283=ORIENTED_EDGE('',*,*,#4006,.F.);
#5284=ORIENTED_EDGE('',*,*,#4007,.F.);
#5285=ORIENTED_EDGE('',*,*,#4008,.F.);
#5286=ORIENTED_EDGE('',*,*,#4009,.F.);
#5287=ORIENTED_EDGE('',*,*,#4010,.T.);
#5288=ORIENTED_EDGE('',*,*,#3998,.T.);
#5289=ORIENTED_EDGE('',*,*,#4011,.F.);
#5290=ORIENTED_EDGE('',*,*,#4003,.F.);
#5291=ORIENTED_EDGE('',*,*,#4012,.T.);
#5292=ORIENTED_EDGE('',*,*,#4009,.T.);
#5293=ORIENTED_EDGE('',*,*,#4012,.F.);
#5294=ORIENTED_EDGE('',*,*,#4002,.F.);
#5295=ORIENTED_EDGE('',*,*,#3999,.F.);
#5296=ORIENTED_EDGE('',*,*,#4010,.F.);
#5297=ORIENTED_EDGE('',*,*,#4013,.T.);
#5298=ORIENTED_EDGE('',*,*,#4006,.T.);
#5299=ORIENTED_EDGE('',*,*,#3997,.T.);
#5300=ORIENTED_EDGE('',*,*,#4001,.T.);
#5301=ORIENTED_EDGE('',*,*,#4014,.T.);
#5302=ORIENTED_EDGE('',*,*,#4015,.F.);
#5303=ORIENTED_EDGE('',*,*,#4016,.T.);
#5304=ORIENTED_EDGE('',*,*,#4017,.F.);
#5305=ORIENTED_EDGE('',*,*,#4018,.F.);
#5306=ORIENTED_EDGE('',*,*,#4019,.F.);
#5307=ORIENTED_EDGE('',*,*,#4018,.T.);
#5308=ORIENTED_EDGE('',*,*,#4020,.F.);
#5309=ORIENTED_EDGE('',*,*,#4021,.F.);
#5310=ORIENTED_EDGE('',*,*,#4022,.F.);
#5311=ORIENTED_EDGE('',*,*,#4021,.T.);
#5312=ORIENTED_EDGE('',*,*,#4023,.F.);
#5313=ORIENTED_EDGE('',*,*,#4024,.F.);
#5314=ORIENTED_EDGE('',*,*,#4025,.F.);
#5315=ORIENTED_EDGE('',*,*,#4024,.T.);
#5316=ORIENTED_EDGE('',*,*,#4026,.F.);
#5317=ORIENTED_EDGE('',*,*,#4016,.F.);
#5318=ORIENTED_EDGE('',*,*,#4025,.T.);
#5319=ORIENTED_EDGE('',*,*,#4015,.T.);
#5320=ORIENTED_EDGE('',*,*,#4019,.T.);
#5321=ORIENTED_EDGE('',*,*,#4022,.T.);
#5322=ORIENTED_EDGE('',*,*,#4008,.T.);
#5323=ORIENTED_EDGE('',*,*,#4027,.F.);
#5324=ORIENTED_EDGE('',*,*,#4004,.T.);
#5325=ORIENTED_EDGE('',*,*,#4011,.T.);
#5326=ORIENTED_EDGE('',*,*,#4028,.F.);
#5327=ORIENTED_EDGE('',*,*,#4017,.T.);
#5328=ORIENTED_EDGE('',*,*,#4026,.T.);
#5329=ORIENTED_EDGE('',*,*,#4023,.T.);
#5330=ORIENTED_EDGE('',*,*,#4020,.T.);
#5331=ORIENTED_EDGE('',*,*,#4007,.T.);
#5332=ORIENTED_EDGE('',*,*,#4014,.F.);
#5333=ORIENTED_EDGE('',*,*,#4005,.T.);
#5334=ORIENTED_EDGE('',*,*,#4027,.T.);
#5335=ORIENTED_EDGE('',*,*,#3995,.T.);
#5336=ORIENTED_EDGE('',*,*,#3996,.T.);
#5337=ORIENTED_EDGE('',*,*,#3989,.T.);
#5338=ORIENTED_EDGE('',*,*,#3987,.T.);
#5339=ORIENTED_EDGE('',*,*,#4013,.F.);
#5340=ORIENTED_EDGE('',*,*,#4029,.T.);
#5341=ORIENTED_EDGE('',*,*,#4028,.T.);
#5342=ORIENTED_EDGE('',*,*,#4029,.F.);
#5343=ORIENTED_EDGE('',*,*,#3992,.T.);
#5344=ORIENTED_EDGE('',*,*,#3993,.T.);
#5345=ORIENTED_EDGE('',*,*,#4030,.F.);
#5346=ORIENTED_EDGE('',*,*,#4031,.T.);
#5347=ORIENTED_EDGE('',*,*,#4032,.F.);
#5348=ORIENTED_EDGE('',*,*,#4033,.F.);
#5349=ORIENTED_EDGE('',*,*,#4034,.T.);
#5350=ORIENTED_EDGE('',*,*,#4035,.F.);
#5351=ORIENTED_EDGE('',*,*,#4036,.F.);
#5352=ORIENTED_EDGE('',*,*,#4034,.F.);
#5353=ORIENTED_EDGE('',*,*,#4037,.F.);
#5354=ORIENTED_EDGE('',*,*,#4038,.F.);
#5355=ORIENTED_EDGE('',*,*,#4031,.F.);
#5356=ORIENTED_EDGE('',*,*,#4039,.F.);
#5357=ORIENTED_EDGE('',*,*,#4037,.T.);
#5358=ORIENTED_EDGE('',*,*,#4033,.T.);
#5359=ORIENTED_EDGE('',*,*,#4040,.F.);
#5360=ORIENTED_EDGE('',*,*,#4041,.T.);
#5361=ORIENTED_EDGE('',*,*,#4042,.F.);
#5362=ORIENTED_EDGE('',*,*,#4043,.F.);
#5363=ORIENTED_EDGE('',*,*,#4044,.F.);
#5364=ORIENTED_EDGE('',*,*,#4045,.T.);
#5365=ORIENTED_EDGE('',*,*,#4046,.F.);
#5366=ORIENTED_EDGE('',*,*,#4041,.F.);
#5367=ORIENTED_EDGE('',*,*,#4047,.F.);
#5368=ORIENTED_EDGE('',*,*,#4048,.F.);
#5369=ORIENTED_EDGE('',*,*,#4049,.F.);
#5370=ORIENTED_EDGE('',*,*,#4045,.F.);
#5371=ORIENTED_EDGE('',*,*,#4050,.T.);
#5372=ORIENTED_EDGE('',*,*,#4042,.T.);
#5373=ORIENTED_EDGE('',*,*,#4046,.T.);
#5374=ORIENTED_EDGE('',*,*,#4049,.T.);
#5375=ORIENTED_EDGE('',*,*,#4051,.T.);
#5376=ORIENTED_EDGE('',*,*,#4043,.T.);
#5377=ORIENTED_EDGE('',*,*,#4051,.F.);
#5378=ORIENTED_EDGE('',*,*,#4048,.T.);
#5379=ORIENTED_EDGE('',*,*,#4052,.T.);
#5380=ORIENTED_EDGE('',*,*,#4038,.T.);
#5381=ORIENTED_EDGE('',*,*,#4039,.T.);
#5382=ORIENTED_EDGE('',*,*,#4032,.T.);
#5383=ORIENTED_EDGE('',*,*,#4030,.T.);
#5384=ORIENTED_EDGE('',*,*,#4053,.F.);
#5385=ORIENTED_EDGE('',*,*,#4054,.T.);
#5386=ORIENTED_EDGE('',*,*,#4055,.F.);
#5387=ORIENTED_EDGE('',*,*,#4054,.F.);
#5388=ORIENTED_EDGE('',*,*,#4056,.F.);
#5389=ORIENTED_EDGE('',*,*,#4057,.F.);
#5390=ORIENTED_EDGE('',*,*,#4058,.F.);
#5391=ORIENTED_EDGE('',*,*,#4059,.T.);
#5392=ORIENTED_EDGE('',*,*,#4059,.F.);
#5393=ORIENTED_EDGE('',*,*,#4060,.T.);
#5394=ORIENTED_EDGE('',*,*,#4061,.F.);
#5395=ORIENTED_EDGE('',*,*,#4062,.T.);
#5396=ORIENTED_EDGE('',*,*,#4053,.T.);
#5397=ORIENTED_EDGE('',*,*,#4058,.T.);
#5398=ORIENTED_EDGE('',*,*,#4063,.F.);
#5399=ORIENTED_EDGE('',*,*,#4064,.F.);
#5400=ORIENTED_EDGE('',*,*,#4060,.F.);
#5401=ORIENTED_EDGE('',*,*,#4065,.T.);
#5402=ORIENTED_EDGE('',*,*,#4066,.F.);
#5403=ORIENTED_EDGE('',*,*,#4063,.T.);
#5404=ORIENTED_EDGE('',*,*,#4057,.T.);
#5405=ORIENTED_EDGE('',*,*,#4055,.T.);
#5406=ORIENTED_EDGE('',*,*,#4056,.T.);
#5407=ORIENTED_EDGE('',*,*,#4062,.F.);
#5408=ORIENTED_EDGE('',*,*,#4067,.F.);
#5409=ORIENTED_EDGE('',*,*,#4065,.F.);
#5410=ORIENTED_EDGE('',*,*,#4050,.F.);
#5411=ORIENTED_EDGE('',*,*,#4068,.T.);
#5412=ORIENTED_EDGE('',*,*,#4069,.T.);
#5413=ORIENTED_EDGE('',*,*,#4068,.F.);
#5414=ORIENTED_EDGE('',*,*,#4035,.T.);
#5415=ORIENTED_EDGE('',*,*,#4036,.T.);
#5416=ORIENTED_EDGE('',*,*,#4064,.T.);
#5417=ORIENTED_EDGE('',*,*,#4066,.T.);
#5418=ORIENTED_EDGE('',*,*,#4067,.T.);
#5419=ORIENTED_EDGE('',*,*,#4061,.T.);
#5420=ORIENTED_EDGE('',*,*,#4069,.F.);
#5421=ORIENTED_EDGE('',*,*,#4040,.T.);
#5422=ORIENTED_EDGE('',*,*,#4052,.F.);
#5423=ORIENTED_EDGE('',*,*,#4047,.T.);
#5424=ORIENTED_EDGE('',*,*,#4044,.T.);
#5425=ORIENTED_EDGE('',*,*,#4070,.F.);
#5426=ORIENTED_EDGE('',*,*,#4071,.T.);
#5427=ORIENTED_EDGE('',*,*,#4072,.F.);
#5428=ORIENTED_EDGE('',*,*,#4071,.F.);
#5429=ORIENTED_EDGE('',*,*,#4070,.T.);
#5430=ORIENTED_EDGE('',*,*,#4073,.T.);
#5431=ORIENTED_EDGE('',*,*,#4073,.F.);
#5432=ORIENTED_EDGE('',*,*,#4074,.T.);
#5433=ORIENTED_EDGE('',*,*,#4075,.T.);
#5434=ORIENTED_EDGE('',*,*,#4074,.F.);
#5435=ORIENTED_EDGE('',*,*,#4076,.F.);
#5436=ORIENTED_EDGE('',*,*,#4077,.T.);
#5437=ORIENTED_EDGE('',*,*,#4078,.T.);
#5438=ORIENTED_EDGE('',*,*,#4077,.F.);
#5439=ORIENTED_EDGE('',*,*,#4076,.T.);
#5440=ORIENTED_EDGE('',*,*,#4072,.T.);
#5441=ORIENTED_EDGE('',*,*,#4078,.F.);
#5442=ORIENTED_EDGE('',*,*,#4075,.F.);
#5443=ORIENTED_EDGE('',*,*,#4079,.F.);
#5444=ORIENTED_EDGE('',*,*,#4080,.T.);
#5445=ORIENTED_EDGE('',*,*,#4081,.T.);
#5446=ORIENTED_EDGE('',*,*,#4080,.F.);
#5447=ORIENTED_EDGE('',*,*,#4081,.F.);
#5448=ORIENTED_EDGE('',*,*,#4082,.F.);
#5449=ORIENTED_EDGE('',*,*,#4083,.F.);
#5450=ORIENTED_EDGE('',*,*,#4084,.T.);
#5451=ORIENTED_EDGE('',*,*,#4082,.T.);
#5452=ORIENTED_EDGE('',*,*,#4084,.F.);
#5453=ORIENTED_EDGE('',*,*,#4085,.F.);
#5454=ORIENTED_EDGE('',*,*,#4086,.T.);
#5455=ORIENTED_EDGE('',*,*,#4087,.T.);
#5456=ORIENTED_EDGE('',*,*,#4086,.F.);
#5457=ORIENTED_EDGE('',*,*,#4085,.T.);
#5458=ORIENTED_EDGE('',*,*,#4083,.T.);
#5459=ORIENTED_EDGE('',*,*,#4087,.F.);
#5460=ORIENTED_EDGE('',*,*,#4079,.T.);
#5461=ORIENTED_EDGE('',*,*,#4088,.F.);
#5462=ORIENTED_EDGE('',*,*,#4089,.F.);
#5463=ORIENTED_EDGE('',*,*,#4090,.F.);
#5464=ORIENTED_EDGE('',*,*,#4091,.F.);
#5465=ORIENTED_EDGE('',*,*,#4092,.F.);
#5466=ORIENTED_EDGE('',*,*,#4093,.F.);
#5467=ORIENTED_EDGE('',*,*,#4094,.F.);
#5468=ORIENTED_EDGE('',*,*,#4095,.F.);
#5469=ORIENTED_EDGE('',*,*,#4092,.T.);
#5470=ORIENTED_EDGE('',*,*,#4096,.T.);
#5471=ORIENTED_EDGE('',*,*,#4097,.T.);
#5472=ORIENTED_EDGE('',*,*,#4098,.T.);
#5473=ORIENTED_EDGE('',*,*,#4091,.T.);
#5474=ORIENTED_EDGE('',*,*,#4099,.F.);
#5475=ORIENTED_EDGE('',*,*,#4100,.T.);
#5476=ORIENTED_EDGE('',*,*,#4096,.F.);
#5477=ORIENTED_EDGE('',*,*,#4090,.T.);
#5478=ORIENTED_EDGE('',*,*,#4101,.T.);
#5479=ORIENTED_EDGE('',*,*,#4102,.T.);
#5480=ORIENTED_EDGE('',*,*,#4099,.T.);
#5481=ORIENTED_EDGE('',*,*,#4089,.T.);
#5482=ORIENTED_EDGE('',*,*,#4103,.F.);
#5483=ORIENTED_EDGE('',*,*,#4104,.T.);
#5484=ORIENTED_EDGE('',*,*,#4101,.F.);
#5485=ORIENTED_EDGE('',*,*,#4097,.F.);
#5486=ORIENTED_EDGE('',*,*,#4100,.F.);
#5487=ORIENTED_EDGE('',*,*,#4102,.F.);
#5488=ORIENTED_EDGE('',*,*,#4104,.F.);
#5489=ORIENTED_EDGE('',*,*,#4105,.F.);
#5490=ORIENTED_EDGE('',*,*,#4106,.F.);
#5491=ORIENTED_EDGE('',*,*,#4107,.F.);
#5492=ORIENTED_EDGE('',*,*,#4108,.F.);
#5493=ORIENTED_EDGE('',*,*,#4088,.T.);
#5494=ORIENTED_EDGE('',*,*,#4109,.T.);
#5495=ORIENTED_EDGE('',*,*,#4105,.T.);
#5496=ORIENTED_EDGE('',*,*,#4103,.T.);
#5497=ORIENTED_EDGE('',*,*,#4095,.T.);
#5498=ORIENTED_EDGE('',*,*,#4110,.F.);
#5499=ORIENTED_EDGE('',*,*,#4106,.T.);
#5500=ORIENTED_EDGE('',*,*,#4109,.F.);
#5501=ORIENTED_EDGE('',*,*,#4094,.T.);
#5502=ORIENTED_EDGE('',*,*,#4111,.T.);
#5503=ORIENTED_EDGE('',*,*,#4107,.T.);
#5504=ORIENTED_EDGE('',*,*,#4110,.T.);
#5505=ORIENTED_EDGE('',*,*,#4093,.T.);
#5506=ORIENTED_EDGE('',*,*,#4098,.F.);
#5507=ORIENTED_EDGE('',*,*,#4108,.T.);
#5508=ORIENTED_EDGE('',*,*,#4111,.F.);
#5509=ORIENTED_EDGE('',*,*,#4112,.F.);
#5510=ORIENTED_EDGE('',*,*,#4113,.T.);
#5511=ORIENTED_EDGE('',*,*,#4114,.T.);
#5512=ORIENTED_EDGE('',*,*,#4115,.F.);
#5513=ORIENTED_EDGE('',*,*,#4116,.F.);
#5514=ORIENTED_EDGE('',*,*,#4117,.T.);
#5515=ORIENTED_EDGE('',*,*,#4118,.T.);
#5516=ORIENTED_EDGE('',*,*,#4113,.F.);
#5517=ORIENTED_EDGE('',*,*,#4119,.F.);
#5518=ORIENTED_EDGE('',*,*,#4120,.T.);
#5519=ORIENTED_EDGE('',*,*,#4121,.T.);
#5520=ORIENTED_EDGE('',*,*,#4117,.F.);
#5521=ORIENTED_EDGE('',*,*,#4122,.F.);
#5522=ORIENTED_EDGE('',*,*,#4123,.T.);
#5523=ORIENTED_EDGE('',*,*,#4124,.T.);
#5524=ORIENTED_EDGE('',*,*,#4120,.F.);
#5525=ORIENTED_EDGE('',*,*,#4125,.F.);
#5526=ORIENTED_EDGE('',*,*,#4126,.T.);
#5527=ORIENTED_EDGE('',*,*,#4127,.T.);
#5528=ORIENTED_EDGE('',*,*,#4123,.F.);
#5529=ORIENTED_EDGE('',*,*,#4128,.F.);
#5530=ORIENTED_EDGE('',*,*,#4115,.T.);
#5531=ORIENTED_EDGE('',*,*,#4129,.T.);
#5532=ORIENTED_EDGE('',*,*,#4126,.F.);
#5533=ORIENTED_EDGE('',*,*,#4129,.F.);
#5534=ORIENTED_EDGE('',*,*,#4114,.F.);
#5535=ORIENTED_EDGE('',*,*,#4118,.F.);
#5536=ORIENTED_EDGE('',*,*,#4121,.F.);
#5537=ORIENTED_EDGE('',*,*,#4124,.F.);
#5538=ORIENTED_EDGE('',*,*,#4127,.F.);
#5539=ORIENTED_EDGE('',*,*,#4130,.F.);
#5540=ORIENTED_EDGE('',*,*,#4112,.T.);
#5541=ORIENTED_EDGE('',*,*,#4128,.T.);
#5542=ORIENTED_EDGE('',*,*,#4125,.T.);
#5543=ORIENTED_EDGE('',*,*,#4122,.T.);
#5544=ORIENTED_EDGE('',*,*,#4119,.T.);
#5545=ORIENTED_EDGE('',*,*,#4116,.T.);
#5546=ORIENTED_EDGE('',*,*,#4131,.F.);
#5547=ORIENTED_EDGE('',*,*,#4132,.T.);
#5548=ORIENTED_EDGE('',*,*,#4130,.T.);
#5549=ORIENTED_EDGE('',*,*,#4132,.F.);
#5550=ORIENTED_EDGE('',*,*,#4133,.F.);
#5551=ORIENTED_EDGE('',*,*,#4134,.T.);
#5552=ORIENTED_EDGE('',*,*,#4131,.T.);
#5553=ORIENTED_EDGE('',*,*,#4134,.F.);
#5554=ORIENTED_EDGE('',*,*,#4135,.F.);
#5555=ORIENTED_EDGE('',*,*,#4136,.T.);
#5556=ORIENTED_EDGE('',*,*,#4133,.T.);
#5557=ORIENTED_EDGE('',*,*,#4136,.F.);
#5558=ORIENTED_EDGE('',*,*,#4135,.T.);
#5559=ORIENTED_EDGE('',*,*,#4137,.F.);
#5560=ORIENTED_EDGE('',*,*,#4138,.F.);
#5561=ORIENTED_EDGE('',*,*,#4139,.T.);
#5562=ORIENTED_EDGE('',*,*,#4140,.F.);
#5563=ORIENTED_EDGE('',*,*,#4141,.F.);
#5564=ORIENTED_EDGE('',*,*,#4139,.F.);
#5565=ORIENTED_EDGE('',*,*,#4140,.T.);
#5566=ORIENTED_EDGE('',*,*,#4141,.T.);
#5567=ORIENTED_EDGE('',*,*,#4142,.T.);
#5568=ORIENTED_EDGE('',*,*,#4143,.T.);
#5569=ORIENTED_EDGE('',*,*,#4142,.F.);
#5570=ORIENTED_EDGE('',*,*,#4144,.T.);
#5571=ORIENTED_EDGE('',*,*,#4145,.T.);
#5572=ORIENTED_EDGE('',*,*,#4146,.F.);
#5573=ORIENTED_EDGE('',*,*,#4145,.F.);
#5574=ORIENTED_EDGE('',*,*,#4146,.T.);
#5575=ORIENTED_EDGE('',*,*,#4147,.T.);
#5576=ORIENTED_EDGE('',*,*,#4148,.F.);
#5577=ORIENTED_EDGE('',*,*,#4147,.F.);
#5578=ORIENTED_EDGE('',*,*,#4143,.F.);
#5579=ORIENTED_EDGE('',*,*,#4148,.T.);
#5580=ORIENTED_EDGE('',*,*,#4149,.F.);
#5581=ORIENTED_EDGE('',*,*,#4150,.T.);
#5582=ORIENTED_EDGE('',*,*,#4137,.T.);
#5583=ORIENTED_EDGE('',*,*,#4138,.T.);
#5584=ORIENTED_EDGE('',*,*,#4150,.F.);
#5585=ORIENTED_EDGE('',*,*,#4149,.T.);
#5586=ORIENTED_EDGE('',*,*,#4151,.F.);
#5587=ORIENTED_EDGE('',*,*,#4151,.T.);
#5588=ORIENTED_EDGE('',*,*,#4152,.T.);
#5589=ORIENTED_EDGE('',*,*,#4144,.F.);
#5590=ORIENTED_EDGE('',*,*,#4152,.F.);
#5591=ORIENTED_EDGE('',*,*,#4153,.F.);
#5592=ORIENTED_EDGE('',*,*,#4154,.F.);
#5593=ORIENTED_EDGE('',*,*,#4155,.T.);
#5594=ORIENTED_EDGE('',*,*,#4156,.F.);
#5595=ORIENTED_EDGE('',*,*,#4157,.F.);
#5596=ORIENTED_EDGE('',*,*,#4155,.F.);
#5597=ORIENTED_EDGE('',*,*,#4158,.T.);
#5598=ORIENTED_EDGE('',*,*,#4159,.T.);
#5599=ORIENTED_EDGE('',*,*,#4156,.T.);
#5600=ORIENTED_EDGE('',*,*,#4157,.T.);
#5601=ORIENTED_EDGE('',*,*,#4159,.F.);
#5602=ORIENTED_EDGE('',*,*,#4160,.F.);
#5603=ORIENTED_EDGE('',*,*,#4161,.T.);
#5604=ORIENTED_EDGE('',*,*,#4162,.F.);
#5605=ORIENTED_EDGE('',*,*,#4163,.T.);
#5606=ORIENTED_EDGE('',*,*,#4160,.T.);
#5607=ORIENTED_EDGE('',*,*,#4163,.F.);
#5608=ORIENTED_EDGE('',*,*,#4164,.F.);
#5609=ORIENTED_EDGE('',*,*,#4165,.T.);
#5610=ORIENTED_EDGE('',*,*,#4162,.T.);
#5611=ORIENTED_EDGE('',*,*,#4165,.F.);
#5612=ORIENTED_EDGE('',*,*,#4166,.F.);
#5613=ORIENTED_EDGE('',*,*,#4167,.T.);
#5614=ORIENTED_EDGE('',*,*,#4164,.T.);
#5615=ORIENTED_EDGE('',*,*,#4167,.F.);
#5616=ORIENTED_EDGE('',*,*,#4166,.T.);
#5617=ORIENTED_EDGE('',*,*,#4158,.F.);
#5618=ORIENTED_EDGE('',*,*,#4153,.T.);
#5619=ORIENTED_EDGE('',*,*,#4154,.T.);
#5620=ORIENTED_EDGE('',*,*,#4168,.T.);
#5621=ORIENTED_EDGE('',*,*,#4161,.F.);
#5622=ORIENTED_EDGE('',*,*,#4168,.F.);
#5623=ORIENTED_EDGE('',*,*,#4169,.T.);
#5624=ORIENTED_EDGE('',*,*,#4169,.F.);
#5625=ORIENTED_EDGE('',*,*,#4170,.T.);
#5626=ORIENTED_EDGE('',*,*,#4170,.F.);
#5627=ORIENTED_EDGE('',*,*,#4171,.T.);
#5628=ORIENTED_EDGE('',*,*,#4171,.F.);
#5629=ORIENTED_EDGE('',*,*,#4172,.T.);
#5630=ORIENTED_EDGE('',*,*,#4172,.F.);
#5631=ORIENTED_EDGE('',*,*,#4173,.T.);
#5632=ORIENTED_EDGE('',*,*,#4173,.F.);
#5633=ORIENTED_EDGE('',*,*,#4174,.T.);
#5634=ORIENTED_EDGE('',*,*,#4174,.F.);
#5635=ORIENTED_EDGE('',*,*,#4175,.T.);
#5636=ORIENTED_EDGE('',*,*,#4175,.F.);
#5637=ORIENTED_EDGE('',*,*,#4176,.T.);
#5638=ORIENTED_EDGE('',*,*,#4176,.F.);
#5639=ORIENTED_EDGE('',*,*,#4177,.F.);
#5640=ORIENTED_EDGE('',*,*,#4178,.F.);
#5641=ORIENTED_EDGE('',*,*,#4179,.F.);
#5642=ORIENTED_EDGE('',*,*,#4180,.F.);
#5643=ORIENTED_EDGE('',*,*,#4179,.T.);
#5644=ORIENTED_EDGE('',*,*,#4181,.F.);
#5645=ORIENTED_EDGE('',*,*,#4182,.T.);
#5646=ORIENTED_EDGE('',*,*,#4183,.F.);
#5647=ORIENTED_EDGE('',*,*,#4184,.T.);
#5648=ORIENTED_EDGE('',*,*,#4185,.F.);
#5649=ORIENTED_EDGE('',*,*,#4186,.T.);
#5650=ORIENTED_EDGE('',*,*,#4187,.T.);
#5651=ORIENTED_EDGE('',*,*,#4188,.F.);
#5652=ORIENTED_EDGE('',*,*,#4187,.F.);
#5653=ORIENTED_EDGE('',*,*,#4189,.T.);
#5654=ORIENTED_EDGE('',*,*,#4190,.F.);
#5655=ORIENTED_EDGE('',*,*,#4191,.T.);
#5656=ORIENTED_EDGE('',*,*,#4192,.F.);
#5657=ORIENTED_EDGE('',*,*,#4193,.T.);
#5658=ORIENTED_EDGE('',*,*,#4194,.F.);
#5659=ORIENTED_EDGE('',*,*,#4195,.T.);
#5660=ORIENTED_EDGE('',*,*,#4196,.F.);
#5661=ORIENTED_EDGE('',*,*,#4197,.T.);
#5662=ORIENTED_EDGE('',*,*,#4198,.F.);
#5663=ORIENTED_EDGE('',*,*,#4178,.T.);
#5664=ORIENTED_EDGE('',*,*,#4199,.T.);
#5665=ORIENTED_EDGE('',*,*,#4200,.T.);
#5666=ORIENTED_EDGE('',*,*,#4181,.T.);
#5667=ORIENTED_EDGE('',*,*,#4201,.F.);
#5668=ORIENTED_EDGE('',*,*,#4202,.F.);
#5669=ORIENTED_EDGE('',*,*,#4182,.F.);
#5670=ORIENTED_EDGE('',*,*,#4200,.F.);
#5671=ORIENTED_EDGE('',*,*,#4202,.T.);
#5672=ORIENTED_EDGE('',*,*,#4203,.T.);
#5673=ORIENTED_EDGE('',*,*,#4204,.T.);
#5674=ORIENTED_EDGE('',*,*,#4183,.T.);
#5675=ORIENTED_EDGE('',*,*,#4205,.F.);
#5676=ORIENTED_EDGE('',*,*,#4206,.F.);
#5677=ORIENTED_EDGE('',*,*,#4184,.F.);
#5678=ORIENTED_EDGE('',*,*,#4204,.F.);
#5679=ORIENTED_EDGE('',*,*,#4206,.T.);
#5680=ORIENTED_EDGE('',*,*,#4207,.T.);
#5681=ORIENTED_EDGE('',*,*,#4208,.T.);
#5682=ORIENTED_EDGE('',*,*,#4185,.T.);
#5683=ORIENTED_EDGE('',*,*,#4209,.F.);
#5684=ORIENTED_EDGE('',*,*,#4210,.F.);
#5685=ORIENTED_EDGE('',*,*,#4189,.F.);
#5686=ORIENTED_EDGE('',*,*,#4186,.F.);
#5687=ORIENTED_EDGE('',*,*,#4208,.F.);
#5688=ORIENTED_EDGE('',*,*,#4211,.F.);
#5689=ORIENTED_EDGE('',*,*,#4210,.T.);
#5690=ORIENTED_EDGE('',*,*,#4212,.T.);
#5691=ORIENTED_EDGE('',*,*,#4213,.T.);
#5692=ORIENTED_EDGE('',*,*,#4190,.T.);
#5693=ORIENTED_EDGE('',*,*,#4214,.F.);
#5694=ORIENTED_EDGE('',*,*,#4215,.F.);
#5695=ORIENTED_EDGE('',*,*,#4191,.F.);
#5696=ORIENTED_EDGE('',*,*,#4213,.F.);
#5697=ORIENTED_EDGE('',*,*,#4215,.T.);
#5698=ORIENTED_EDGE('',*,*,#4216,.T.);
#5699=ORIENTED_EDGE('',*,*,#4217,.T.);
#5700=ORIENTED_EDGE('',*,*,#4192,.T.);
#5701=ORIENTED_EDGE('',*,*,#4218,.F.);
#5702=ORIENTED_EDGE('',*,*,#4219,.F.);
#5703=ORIENTED_EDGE('',*,*,#4193,.F.);
#5704=ORIENTED_EDGE('',*,*,#4217,.F.);
#5705=ORIENTED_EDGE('',*,*,#4219,.T.);
#5706=ORIENTED_EDGE('',*,*,#4220,.T.);
#5707=ORIENTED_EDGE('',*,*,#4221,.T.);
#5708=ORIENTED_EDGE('',*,*,#4194,.T.);
#5709=ORIENTED_EDGE('',*,*,#4195,.F.);
#5710=ORIENTED_EDGE('',*,*,#4221,.F.);
#5711=ORIENTED_EDGE('',*,*,#4222,.F.);
#5712=ORIENTED_EDGE('',*,*,#4223,.F.);
#5713=ORIENTED_EDGE('',*,*,#4224,.F.);
#5714=ORIENTED_EDGE('',*,*,#4225,.T.);
#5715=ORIENTED_EDGE('',*,*,#4211,.T.);
#5716=ORIENTED_EDGE('',*,*,#4207,.F.);
#5717=ORIENTED_EDGE('',*,*,#4205,.T.);
#5718=ORIENTED_EDGE('',*,*,#4203,.F.);
#5719=ORIENTED_EDGE('',*,*,#4201,.T.);
#5720=ORIENTED_EDGE('',*,*,#4199,.F.);
#5721=ORIENTED_EDGE('',*,*,#4177,.T.);
#5722=ORIENTED_EDGE('',*,*,#4226,.F.);
#5723=ORIENTED_EDGE('',*,*,#4227,.T.);
#5724=ORIENTED_EDGE('',*,*,#4228,.F.);
#5725=ORIENTED_EDGE('',*,*,#4222,.T.);
#5726=ORIENTED_EDGE('',*,*,#4220,.F.);
#5727=ORIENTED_EDGE('',*,*,#4218,.T.);
#5728=ORIENTED_EDGE('',*,*,#4216,.F.);
#5729=ORIENTED_EDGE('',*,*,#4214,.T.);
#5730=ORIENTED_EDGE('',*,*,#4212,.F.);
#5731=ORIENTED_EDGE('',*,*,#4209,.T.);
#5732=ORIENTED_EDGE('',*,*,#4225,.F.);
#5733=ORIENTED_EDGE('',*,*,#4180,.T.);
#5734=ORIENTED_EDGE('',*,*,#4198,.T.);
#5735=ORIENTED_EDGE('',*,*,#4229,.T.);
#5736=ORIENTED_EDGE('',*,*,#4226,.T.);
#5737=ORIENTED_EDGE('',*,*,#4197,.F.);
#5738=ORIENTED_EDGE('',*,*,#4230,.F.);
#5739=ORIENTED_EDGE('',*,*,#4227,.F.);
#5740=ORIENTED_EDGE('',*,*,#4229,.F.);
#5741=ORIENTED_EDGE('',*,*,#4188,.T.);
#5742=ORIENTED_EDGE('',*,*,#4224,.T.);
#5743=ORIENTED_EDGE('',*,*,#4223,.T.);
#5744=ORIENTED_EDGE('',*,*,#4228,.T.);
#5745=ORIENTED_EDGE('',*,*,#4230,.T.);
#5746=ORIENTED_EDGE('',*,*,#4196,.T.);
#5747=ORIENTED_EDGE('',*,*,#4231,.F.);
#5748=ORIENTED_EDGE('',*,*,#4232,.T.);
#5749=ORIENTED_EDGE('',*,*,#4233,.F.);
#5750=ORIENTED_EDGE('',*,*,#4234,.T.);
#5751=ORIENTED_EDGE('',*,*,#4231,.T.);
#5752=ORIENTED_EDGE('',*,*,#4234,.F.);
#5753=ORIENTED_EDGE('',*,*,#4233,.T.);
#5754=ORIENTED_EDGE('',*,*,#4235,.F.);
#5755=ORIENTED_EDGE('',*,*,#4235,.T.);
#5756=ORIENTED_EDGE('',*,*,#4236,.T.);
#5757=ORIENTED_EDGE('',*,*,#4232,.F.);
#5758=ORIENTED_EDGE('',*,*,#4236,.F.);
#5759=ORIENTED_EDGE('',*,*,#4237,.F.);
#5760=ORIENTED_EDGE('',*,*,#4238,.T.);
#5761=ORIENTED_EDGE('',*,*,#4239,.F.);
#5762=ORIENTED_EDGE('',*,*,#4240,.T.);
#5763=ORIENTED_EDGE('',*,*,#4237,.T.);
#5764=ORIENTED_EDGE('',*,*,#4240,.F.);
#5765=ORIENTED_EDGE('',*,*,#4239,.T.);
#5766=ORIENTED_EDGE('',*,*,#4241,.F.);
#5767=ORIENTED_EDGE('',*,*,#4241,.T.);
#5768=ORIENTED_EDGE('',*,*,#4242,.T.);
#5769=ORIENTED_EDGE('',*,*,#4238,.F.);
#5770=ORIENTED_EDGE('',*,*,#4242,.F.);
#5771=ORIENTED_EDGE('',*,*,#4243,.F.);
#5772=ORIENTED_EDGE('',*,*,#4244,.T.);
#5773=ORIENTED_EDGE('',*,*,#4245,.F.);
#5774=ORIENTED_EDGE('',*,*,#4244,.F.);
#5775=ORIENTED_EDGE('',*,*,#4246,.F.);
#5776=ORIENTED_EDGE('',*,*,#4247,.T.);
#5777=ORIENTED_EDGE('',*,*,#4248,.F.);
#5778=ORIENTED_EDGE('',*,*,#4247,.F.);
#5779=ORIENTED_EDGE('',*,*,#4249,.F.);
#5780=ORIENTED_EDGE('',*,*,#4250,.T.);
#5781=ORIENTED_EDGE('',*,*,#4251,.F.);
#5782=ORIENTED_EDGE('',*,*,#4250,.F.);
#5783=ORIENTED_EDGE('',*,*,#4252,.F.);
#5784=ORIENTED_EDGE('',*,*,#4253,.T.);
#5785=ORIENTED_EDGE('',*,*,#4254,.F.);
#5786=ORIENTED_EDGE('',*,*,#4255,.F.);
#5787=ORIENTED_EDGE('',*,*,#4245,.T.);
#5788=ORIENTED_EDGE('',*,*,#4256,.F.);
#5789=ORIENTED_EDGE('',*,*,#4257,.T.);
#5790=ORIENTED_EDGE('',*,*,#4258,.F.);
#5791=ORIENTED_EDGE('',*,*,#4259,.F.);
#5792=ORIENTED_EDGE('',*,*,#4258,.T.);
#5793=ORIENTED_EDGE('',*,*,#4260,.T.);
#5794=ORIENTED_EDGE('',*,*,#4261,.T.);
#5795=ORIENTED_EDGE('',*,*,#4262,.T.);
#5796=ORIENTED_EDGE('',*,*,#4251,.T.);
#5797=ORIENTED_EDGE('',*,*,#4254,.T.);
#5798=ORIENTED_EDGE('',*,*,#4263,.T.);
#5799=ORIENTED_EDGE('',*,*,#4256,.T.);
#5800=ORIENTED_EDGE('',*,*,#4264,.T.);
#5801=ORIENTED_EDGE('',*,*,#4249,.T.);
#5802=ORIENTED_EDGE('',*,*,#4252,.T.);
#5803=ORIENTED_EDGE('',*,*,#4265,.T.);
#5804=ORIENTED_EDGE('',*,*,#4266,.T.);
#5805=ORIENTED_EDGE('',*,*,#4267,.T.);
#5806=ORIENTED_EDGE('',*,*,#4248,.T.);
#5807=ORIENTED_EDGE('',*,*,#4268,.F.);
#5808=ORIENTED_EDGE('',*,*,#4269,.T.);
#5809=ORIENTED_EDGE('',*,*,#4265,.F.);
#5810=ORIENTED_EDGE('',*,*,#4255,.T.);
#5811=ORIENTED_EDGE('',*,*,#4264,.F.);
#5812=ORIENTED_EDGE('',*,*,#4259,.T.);
#5813=ORIENTED_EDGE('',*,*,#4262,.F.);
#5814=ORIENTED_EDGE('',*,*,#4270,.F.);
#5815=ORIENTED_EDGE('',*,*,#4271,.F.);
#5816=ORIENTED_EDGE('',*,*,#4270,.T.);
#5817=ORIENTED_EDGE('',*,*,#4261,.F.);
#5818=ORIENTED_EDGE('',*,*,#4272,.F.);
#5819=ORIENTED_EDGE('',*,*,#4243,.T.);
#5820=ORIENTED_EDGE('',*,*,#4273,.F.);
#5821=ORIENTED_EDGE('',*,*,#4272,.T.);
#5822=ORIENTED_EDGE('',*,*,#4260,.F.);
#5823=ORIENTED_EDGE('',*,*,#4257,.F.);
#5824=ORIENTED_EDGE('',*,*,#4263,.F.);
#5825=ORIENTED_EDGE('',*,*,#4253,.F.);
#5826=ORIENTED_EDGE('',*,*,#4267,.F.);
#5827=ORIENTED_EDGE('',*,*,#4274,.F.);
#5828=ORIENTED_EDGE('',*,*,#4275,.F.);
#5829=ORIENTED_EDGE('',*,*,#4274,.T.);
#5830=ORIENTED_EDGE('',*,*,#4266,.F.);
#5831=ORIENTED_EDGE('',*,*,#4269,.F.);
#5832=ORIENTED_EDGE('',*,*,#4275,.T.);
#5833=ORIENTED_EDGE('',*,*,#4268,.T.);
#5834=ORIENTED_EDGE('',*,*,#4271,.T.);
#5835=ORIENTED_EDGE('',*,*,#4273,.T.);
#5836=ORIENTED_EDGE('',*,*,#4246,.T.);
#5837=ORIENTED_EDGE('',*,*,#4276,.F.);
#5838=ORIENTED_EDGE('',*,*,#4277,.T.);
#5839=ORIENTED_EDGE('',*,*,#4278,.F.);
#5840=ORIENTED_EDGE('',*,*,#4277,.F.);
#5841=ORIENTED_EDGE('',*,*,#4276,.T.);
#5842=ORIENTED_EDGE('',*,*,#4279,.F.);
#5843=ORIENTED_EDGE('',*,*,#4280,.T.);
#5844=ORIENTED_EDGE('',*,*,#4281,.T.);
#5845=ORIENTED_EDGE('',*,*,#4280,.F.);
#5846=ORIENTED_EDGE('',*,*,#4281,.F.);
#5847=ORIENTED_EDGE('',*,*,#4282,.F.);
#5848=ORIENTED_EDGE('',*,*,#4283,.T.);
#5849=ORIENTED_EDGE('',*,*,#4284,.T.);
#5850=ORIENTED_EDGE('',*,*,#4283,.F.);
#5851=ORIENTED_EDGE('',*,*,#4282,.T.);
#5852=ORIENTED_EDGE('',*,*,#4278,.T.);
#5853=ORIENTED_EDGE('',*,*,#4284,.F.);
#5854=ORIENTED_EDGE('',*,*,#4279,.T.);
#5855=ORIENTED_EDGE('',*,*,#4285,.F.);
#5856=ORIENTED_EDGE('',*,*,#4286,.T.);
#5857=ORIENTED_EDGE('',*,*,#4287,.T.);
#5858=ORIENTED_EDGE('',*,*,#4286,.F.);
#5859=ORIENTED_EDGE('',*,*,#4288,.F.);
#5860=ORIENTED_EDGE('',*,*,#4289,.T.);
#5861=ORIENTED_EDGE('',*,*,#4290,.T.);
#5862=ORIENTED_EDGE('',*,*,#4289,.F.);
#5863=ORIENTED_EDGE('',*,*,#4288,.T.);
#5864=ORIENTED_EDGE('',*,*,#4285,.T.);
#5865=ORIENTED_EDGE('',*,*,#4290,.F.);
#5866=ORIENTED_EDGE('',*,*,#4287,.F.);
#5867=ORIENTED_EDGE('',*,*,#4291,.F.);
#5868=ORIENTED_EDGE('',*,*,#4292,.T.);
#5869=ORIENTED_EDGE('',*,*,#4293,.T.);
#5870=ORIENTED_EDGE('',*,*,#4292,.F.);
#5871=ORIENTED_EDGE('',*,*,#4294,.F.);
#5872=ORIENTED_EDGE('',*,*,#4295,.T.);
#5873=ORIENTED_EDGE('',*,*,#4296,.T.);
#5874=ORIENTED_EDGE('',*,*,#4295,.F.);
#5875=ORIENTED_EDGE('',*,*,#4294,.T.);
#5876=ORIENTED_EDGE('',*,*,#4291,.T.);
#5877=ORIENTED_EDGE('',*,*,#4296,.F.);
#5878=ORIENTED_EDGE('',*,*,#4293,.F.);
#5879=ORIENTED_EDGE('',*,*,#4297,.F.);
#5880=ORIENTED_EDGE('',*,*,#4298,.T.);
#5881=ORIENTED_EDGE('',*,*,#4299,.T.);
#5882=ORIENTED_EDGE('',*,*,#4298,.F.);
#5883=ORIENTED_EDGE('',*,*,#4300,.F.);
#5884=ORIENTED_EDGE('',*,*,#4301,.T.);
#5885=ORIENTED_EDGE('',*,*,#4302,.T.);
#5886=ORIENTED_EDGE('',*,*,#4301,.F.);
#5887=ORIENTED_EDGE('',*,*,#4300,.T.);
#5888=ORIENTED_EDGE('',*,*,#4297,.T.);
#5889=ORIENTED_EDGE('',*,*,#4302,.F.);
#5890=ORIENTED_EDGE('',*,*,#4299,.F.);
#5891=ORIENTED_EDGE('',*,*,#4303,.F.);
#5892=ORIENTED_EDGE('',*,*,#4304,.T.);
#5893=ORIENTED_EDGE('',*,*,#4305,.T.);
#5894=ORIENTED_EDGE('',*,*,#4304,.F.);
#5895=ORIENTED_EDGE('',*,*,#4306,.F.);
#5896=ORIENTED_EDGE('',*,*,#4307,.T.);
#5897=ORIENTED_EDGE('',*,*,#4308,.T.);
#5898=ORIENTED_EDGE('',*,*,#4307,.F.);
#5899=ORIENTED_EDGE('',*,*,#4306,.T.);
#5900=ORIENTED_EDGE('',*,*,#4303,.T.);
#5901=ORIENTED_EDGE('',*,*,#4308,.F.);
#5902=ORIENTED_EDGE('',*,*,#4305,.F.);
#5903=ORIENTED_EDGE('',*,*,#4309,.F.);
#5904=ORIENTED_EDGE('',*,*,#4310,.T.);
#5905=ORIENTED_EDGE('',*,*,#4311,.T.);
#5906=ORIENTED_EDGE('',*,*,#4310,.F.);
#5907=ORIENTED_EDGE('',*,*,#4312,.F.);
#5908=ORIENTED_EDGE('',*,*,#4313,.T.);
#5909=ORIENTED_EDGE('',*,*,#4314,.T.);
#5910=ORIENTED_EDGE('',*,*,#4313,.F.);
#5911=ORIENTED_EDGE('',*,*,#4312,.T.);
#5912=ORIENTED_EDGE('',*,*,#4309,.T.);
#5913=ORIENTED_EDGE('',*,*,#4314,.F.);
#5914=ORIENTED_EDGE('',*,*,#4311,.F.);
#5915=ORIENTED_EDGE('',*,*,#4315,.F.);
#5916=ORIENTED_EDGE('',*,*,#4316,.T.);
#5917=ORIENTED_EDGE('',*,*,#4317,.T.);
#5918=ORIENTED_EDGE('',*,*,#4316,.F.);
#5919=ORIENTED_EDGE('',*,*,#4318,.F.);
#5920=ORIENTED_EDGE('',*,*,#4319,.T.);
#5921=ORIENTED_EDGE('',*,*,#4320,.T.);
#5922=ORIENTED_EDGE('',*,*,#4319,.F.);
#5923=ORIENTED_EDGE('',*,*,#4318,.T.);
#5924=ORIENTED_EDGE('',*,*,#4315,.T.);
#5925=ORIENTED_EDGE('',*,*,#4320,.F.);
#5926=ORIENTED_EDGE('',*,*,#4317,.F.);
#5927=ORIENTED_EDGE('',*,*,#4321,.T.);
#5928=ORIENTED_EDGE('',*,*,#4322,.T.);
#5929=ORIENTED_EDGE('',*,*,#4323,.T.);
#5930=ORIENTED_EDGE('',*,*,#4324,.F.);
#5931=ORIENTED_EDGE('',*,*,#4325,.T.);
#5932=ORIENTED_EDGE('',*,*,#4326,.T.);
#5933=ORIENTED_EDGE('',*,*,#4327,.T.);
#5934=ORIENTED_EDGE('',*,*,#4322,.F.);
#5935=ORIENTED_EDGE('',*,*,#4328,.T.);
#5936=ORIENTED_EDGE('',*,*,#4329,.T.);
#5937=ORIENTED_EDGE('',*,*,#4330,.T.);
#5938=ORIENTED_EDGE('',*,*,#4326,.F.);
#5939=ORIENTED_EDGE('',*,*,#4331,.T.);
#5940=ORIENTED_EDGE('',*,*,#4332,.T.);
#5941=ORIENTED_EDGE('',*,*,#4333,.T.);
#5942=ORIENTED_EDGE('',*,*,#4329,.F.);
#5943=ORIENTED_EDGE('',*,*,#4334,.T.);
#5944=ORIENTED_EDGE('',*,*,#4335,.T.);
#5945=ORIENTED_EDGE('',*,*,#4336,.T.);
#5946=ORIENTED_EDGE('',*,*,#4332,.F.);
#5947=ORIENTED_EDGE('',*,*,#4337,.T.);
#5948=ORIENTED_EDGE('',*,*,#4324,.T.);
#5949=ORIENTED_EDGE('',*,*,#4338,.T.);
#5950=ORIENTED_EDGE('',*,*,#4335,.F.);
#5951=ORIENTED_EDGE('',*,*,#4337,.F.);
#5952=ORIENTED_EDGE('',*,*,#4334,.F.);
#5953=ORIENTED_EDGE('',*,*,#4331,.F.);
#5954=ORIENTED_EDGE('',*,*,#4328,.F.);
#5955=ORIENTED_EDGE('',*,*,#4325,.F.);
#5956=ORIENTED_EDGE('',*,*,#4321,.F.);
#5957=ORIENTED_EDGE('',*,*,#4338,.F.);
#5958=ORIENTED_EDGE('',*,*,#4323,.F.);
#5959=ORIENTED_EDGE('',*,*,#4327,.F.);
#5960=ORIENTED_EDGE('',*,*,#4330,.F.);
#5961=ORIENTED_EDGE('',*,*,#4333,.F.);
#5962=ORIENTED_EDGE('',*,*,#4336,.F.);
#5963=ORIENTED_EDGE('',*,*,#4339,.F.);
#5964=ORIENTED_EDGE('',*,*,#4340,.F.);
#5965=ORIENTED_EDGE('',*,*,#4341,.F.);
#5966=ORIENTED_EDGE('',*,*,#4342,.T.);
#5967=ORIENTED_EDGE('',*,*,#4340,.T.);
#5968=ORIENTED_EDGE('',*,*,#4342,.F.);
#5969=ORIENTED_EDGE('',*,*,#4343,.F.);
#5970=ORIENTED_EDGE('',*,*,#4344,.T.);
#5971=ORIENTED_EDGE('',*,*,#4341,.T.);
#5972=ORIENTED_EDGE('',*,*,#4344,.F.);
#5973=ORIENTED_EDGE('',*,*,#4345,.F.);
#5974=ORIENTED_EDGE('',*,*,#4346,.T.);
#5975=ORIENTED_EDGE('',*,*,#4343,.T.);
#5976=ORIENTED_EDGE('',*,*,#4346,.F.);
#5977=ORIENTED_EDGE('',*,*,#4345,.T.);
#5978=ORIENTED_EDGE('',*,*,#4347,.F.);
#5979=ORIENTED_EDGE('',*,*,#4348,.F.);
#5980=ORIENTED_EDGE('',*,*,#4349,.T.);
#5981=ORIENTED_EDGE('',*,*,#4347,.T.);
#5982=ORIENTED_EDGE('',*,*,#4349,.F.);
#5983=ORIENTED_EDGE('',*,*,#4339,.T.);
#5984=ORIENTED_EDGE('',*,*,#4350,.T.);
#5985=ORIENTED_EDGE('',*,*,#4348,.T.);
#5986=ORIENTED_EDGE('',*,*,#4350,.F.);
#5987=CYLINDRICAL_SURFACE('',#6963,0.25);
#5988=CYLINDRICAL_SURFACE('',#6966,0.25);
#5989=CYLINDRICAL_SURFACE('',#6969,0.25);
#5990=CYLINDRICAL_SURFACE('',#6972,0.25);
#5991=CYLINDRICAL_SURFACE('',#6982,0.165);
#5992=CYLINDRICAL_SURFACE('',#6986,0.165);
#5993=CYLINDRICAL_SURFACE('',#6990,0.165);
#5994=CYLINDRICAL_SURFACE('',#6994,0.165);
#5995=CYLINDRICAL_SURFACE('',#6998,0.165);
#5996=CYLINDRICAL_SURFACE('',#7002,0.165);
#5997=CYLINDRICAL_SURFACE('',#7006,0.165);
#5998=CYLINDRICAL_SURFACE('',#7010,0.165);
#5999=CYLINDRICAL_SURFACE('',#7014,0.6);
#6000=CYLINDRICAL_SURFACE('',#7017,0.6);
#6001=CYLINDRICAL_SURFACE('',#7022,0.6);
#6002=CYLINDRICAL_SURFACE('',#7025,0.6);
#6003=CYLINDRICAL_SURFACE('',#7030,0.6);
#6004=CYLINDRICAL_SURFACE('',#7033,0.6);
#6005=CYLINDRICAL_SURFACE('',#7038,0.6);
#6006=CYLINDRICAL_SURFACE('',#7041,0.6);
#6007=CYLINDRICAL_SURFACE('',#7058,0.33);
#6008=CYLINDRICAL_SURFACE('',#7060,0.33);
#6009=CYLINDRICAL_SURFACE('',#7062,0.33);
#6010=CYLINDRICAL_SURFACE('',#7064,0.33);
#6011=CYLINDRICAL_SURFACE('',#7076,2.6);
#6012=CYLINDRICAL_SURFACE('',#7079,4.);
#6013=CYLINDRICAL_SURFACE('',#7085,2.);
#6014=CYLINDRICAL_SURFACE('',#7088,2.59);
#6015=CYLINDRICAL_SURFACE('',#7094,0.225);
#6016=CYLINDRICAL_SURFACE('',#7097,0.225);
#6017=CYLINDRICAL_SURFACE('',#7100,0.225);
#6018=CYLINDRICAL_SURFACE('',#7103,0.225);
#6019=CYLINDRICAL_SURFACE('',#7106,2.59);
#6020=CYLINDRICAL_SURFACE('',#7111,2.);
#6021=CYLINDRICAL_SURFACE('',#7113,4.);
#6022=CYLINDRICAL_SURFACE('',#7119,0.225);
#6023=CYLINDRICAL_SURFACE('',#7122,0.225);
#6024=CYLINDRICAL_SURFACE('',#7125,0.225);
#6025=CYLINDRICAL_SURFACE('',#7128,0.225);
#6026=CYLINDRICAL_SURFACE('',#7131,2.59);
#6027=CYLINDRICAL_SURFACE('',#7136,2.);
#6028=CYLINDRICAL_SURFACE('',#7138,4.);
#6029=CYLINDRICAL_SURFACE('',#7165,1.88531);
#6030=CYLINDRICAL_SURFACE('',#7167,1.25);
#6031=CYLINDRICAL_SURFACE('',#7173,1.88531);
#6032=CYLINDRICAL_SURFACE('',#7185,1.96469);
#6033=CYLINDRICAL_SURFACE('',#7192,2.6);
#6034=CYLINDRICAL_SURFACE('',#7197,1.96469);
#6035=CYLINDRICAL_SURFACE('',#7221,1.956752);
#6036=CYLINDRICAL_SURFACE('',#7269,1.893248);
#6037=CYLINDRICAL_SURFACE('',#7283,1.95469);
#6038=CYLINDRICAL_SURFACE('',#7287,1.90031);
#6039=CYLINDRICAL_SURFACE('',#7291,1.95469);
#6040=CYLINDRICAL_SURFACE('',#7295,1.90031);
#6041=CYLINDRICAL_SURFACE('',#7306,0.5);
#6042=CYLINDRICAL_SURFACE('',#7314,0.2942);
#6043=CYLINDRICAL_SURFACE('',#7332,0.35);
#6044=CYLINDRICAL_SURFACE('',#7340,0.1954);
#6045=CYLINDRICAL_SURFACE('',#7396,1.6);
#6046=CYLINDRICAL_SURFACE('',#7397,1.25);
#6047=CYLINDRICAL_SURFACE('',#7399,1.25);
#6048=CYLINDRICAL_SURFACE('',#7404,1.255);
#6049=CYLINDRICAL_SURFACE('',#7407,1.7);
#6050=CYLINDRICAL_SURFACE('',#7415,0.21);
#6051=CYLINDRICAL_SURFACE('',#7419,1.255);
#6052=CYLINDRICAL_SURFACE('',#7422,1.8);
#6053=CYLINDRICAL_SURFACE('',#7430,0.21);
#6054=CYLINDRICAL_SURFACE('',#7451,1.25);
#6055=CYLINDRICAL_SURFACE('',#7452,2.);
#6056=CYLINDRICAL_SURFACE('',#7456,0.21);
#6057=CYLINDRICAL_SURFACE('',#7466,1.25);
#6058=CYLINDRICAL_SURFACE('',#7468,1.5);
#6059=CYLINDRICAL_SURFACE('',#7471,2.);
#6060=CYLINDRICAL_SURFACE('',#7480,2.5);
#6061=CYLINDRICAL_SURFACE('',#7484,1.5);
#6062=CYLINDRICAL_SURFACE('',#7489,1.1);
#6063=CYLINDRICAL_SURFACE('',#7491,2.);
#6064=CYLINDRICAL_SURFACE('',#7497,1.5);
#6065=CYLINDRICAL_SURFACE('',#7502,1.1);
#6066=CYLINDRICAL_SURFACE('',#7504,2.);
#6067=CYLINDRICAL_SURFACE('',#7532,0.24505);
#6068=CYLINDRICAL_SURFACE('',#7545,0.976185);
#6069=CYLINDRICAL_SURFACE('',#7547,0.5);
#6070=CYLINDRICAL_SURFACE('',#7553,0.976185);
#6071=CYLINDRICAL_SURFACE('',#7565,1.023815);
#6072=CYLINDRICAL_SURFACE('',#7572,1.5);
#6073=CYLINDRICAL_SURFACE('',#7577,1.023815);
#6074=CYLINDRICAL_SURFACE('',#7599,1.019052);
#6075=CYLINDRICAL_SURFACE('',#7639,0.980948);
#6076=CYLINDRICAL_SURFACE('',#7653,1.013815);
#6077=CYLINDRICAL_SURFACE('',#7657,0.991185);
#6078=CYLINDRICAL_SURFACE('',#7661,1.013815);
#6079=CYLINDRICAL_SURFACE('',#7665,0.991185);
#6080=CYLINDRICAL_SURFACE('',#7686,0.329999999999998);
#6081=CYLINDRICAL_SURFACE('',#7689,0.505000000000003);
#6082=CYLINDRICAL_SURFACE('',#7692,0.505000000000003);
#6083=CYLINDRICAL_SURFACE('',#7706,0.164999999999999);
#6084=CYLINDRICAL_SURFACE('',#7710,0.164999999999999);
#6085=CYLINDRICAL_SURFACE('',#7714,0.5);
#6086=CYLINDRICAL_SURFACE('',#7720,0.505000000000003);
#6087=CYLINDRICAL_SURFACE('',#7723,0.700000000000003);
#6088=CYLINDRICAL_SURFACE('',#7729,0.505000000000003);
#6089=CYLINDRICAL_SURFACE('',#7732,0.700000000000003);
#6090=CYLINDRICAL_SURFACE('',#7738,0.505000000000003);
#6091=CYLINDRICAL_SURFACE('',#7741,0.700000000000003);
#6092=CYLINDRICAL_SURFACE('',#7747,0.505000000000003);
#6093=CYLINDRICAL_SURFACE('',#7750,0.700000000000003);
#6094=CYLINDRICAL_SURFACE('',#7756,0.225000000000001);
#6095=CYLINDRICAL_SURFACE('',#7759,0.799999999999997);
#6096=CYLINDRICAL_SURFACE('',#7765,0.225000000000001);
#6097=CYLINDRICAL_SURFACE('',#7768,0.799999999999997);
#6098=CYLINDRICAL_SURFACE('',#7788,0.35);
#6099=CYLINDRICAL_SURFACE('',#7796,0.1954);
#6100=ADVANCED_FACE('',(#875),#5987,.F.);
#6101=ADVANCED_FACE('',(#876),#5988,.F.);
#6102=ADVANCED_FACE('',(#877),#5989,.F.);
#6103=ADVANCED_FACE('',(#878),#5990,.F.);
#6104=ADVANCED_FACE('',(#879),#652,.T.);
#6105=ADVANCED_FACE('',(#880),#653,.T.);
#6106=ADVANCED_FACE('',(#881),#654,.T.);
#6107=ADVANCED_FACE('',(#882),#655,.T.);
#6108=ADVANCED_FACE('',(#883,#531,#532,#533,#534),#656,.T.);
#6109=ADVANCED_FACE('',(#884,#535,#536,#537,#538),#657,.F.);
#6110=ADVANCED_FACE('',(#885),#5991,.F.);
#6111=ADVANCED_FACE('',(#886),#658,.T.);
#6112=ADVANCED_FACE('',(#887),#5992,.F.);
#6113=ADVANCED_FACE('',(#888),#659,.T.);
#6114=ADVANCED_FACE('',(#889),#5993,.F.);
#6115=ADVANCED_FACE('',(#890),#660,.T.);
#6116=ADVANCED_FACE('',(#891),#5994,.F.);
#6117=ADVANCED_FACE('',(#892),#661,.T.);
#6118=ADVANCED_FACE('',(#893),#5995,.F.);
#6119=ADVANCED_FACE('',(#894),#662,.F.);
#6120=ADVANCED_FACE('',(#895),#5996,.F.);
#6121=ADVANCED_FACE('',(#896),#663,.F.);
#6122=ADVANCED_FACE('',(#897),#5997,.F.);
#6123=ADVANCED_FACE('',(#898),#664,.F.);
#6124=ADVANCED_FACE('',(#899),#5998,.F.);
#6125=ADVANCED_FACE('',(#900),#665,.F.);
#6126=ADVANCED_FACE('',(#901),#5999,.F.);
#6127=ADVANCED_FACE('',(#902),#6000,.F.);
#6128=ADVANCED_FACE('',(#903,#539),#666,.T.);
#6129=ADVANCED_FACE('',(#904),#6001,.F.);
#6130=ADVANCED_FACE('',(#905),#6002,.F.);
#6131=ADVANCED_FACE('',(#906,#540),#667,.T.);
#6132=ADVANCED_FACE('',(#907),#6003,.F.);
#6133=ADVANCED_FACE('',(#908),#6004,.F.);
#6134=ADVANCED_FACE('',(#909,#541),#668,.T.);
#6135=ADVANCED_FACE('',(#910),#6005,.F.);
#6136=ADVANCED_FACE('',(#911),#6006,.F.);
#6137=ADVANCED_FACE('',(#912,#542),#669,.T.);
#6138=ADVANCED_FACE('',(#913),#670,.T.);
#6139=ADVANCED_FACE('',(#914),#671,.T.);
#6140=ADVANCED_FACE('',(#915),#672,.T.);
#6141=ADVANCED_FACE('',(#916),#673,.T.);
#6142=ADVANCED_FACE('',(#917),#674,.T.);
#6143=ADVANCED_FACE('',(#918),#675,.T.);
#6144=ADVANCED_FACE('',(#919),#676,.T.);
#6145=ADVANCED_FACE('',(#920),#677,.T.);
#6146=ADVANCED_FACE('',(#921),#678,.T.);
#6147=ADVANCED_FACE('',(#922),#679,.T.);
#6148=ADVANCED_FACE('',(#923),#6007,.F.);
#6149=ADVANCED_FACE('',(#924),#6008,.F.);
#6150=ADVANCED_FACE('',(#925),#6009,.F.);
#6151=ADVANCED_FACE('',(#926),#6010,.F.);
#6152=ADVANCED_FACE('',(#927),#680,.T.);
#6153=ADVANCED_FACE('',(#928,#543,#544),#681,.T.);
#6154=ADVANCED_FACE('',(#929),#682,.T.);
#6155=ADVANCED_FACE('',(#930),#683,.F.);
#6156=ADVANCED_FACE('',(#931),#684,.T.);
#6157=ADVANCED_FACE('',(#932,#545,#546),#685,.T.);
#6158=ADVANCED_FACE('',(#933),#686,.T.);
#6159=ADVANCED_FACE('',(#934),#687,.F.);
#6160=ADVANCED_FACE('',(#935),#6011,.F.);
#6161=ADVANCED_FACE('',(#936,#547,#548),#6012,.T.);
#6162=ADVANCED_FACE('',(#937,#549,#550,#551,#552,#553),#688,.T.);
#6163=ADVANCED_FACE('',(#938,#554,#555,#556,#557,#558),#689,.F.);
#6164=ADVANCED_FACE('',(#939),#6013,.F.);
#6165=ADVANCED_FACE('',(#940),#6014,.T.);
#6166=ADVANCED_FACE('',(#941,#559),#690,.T.);
#6167=ADVANCED_FACE('',(#942,#560),#691,.F.);
#6168=ADVANCED_FACE('',(#943),#6015,.F.);
#6169=ADVANCED_FACE('',(#944),#6016,.F.);
#6170=ADVANCED_FACE('',(#945),#6017,.F.);
#6171=ADVANCED_FACE('',(#946),#6018,.F.);
#6172=ADVANCED_FACE('',(#947),#6019,.T.);
#6173=ADVANCED_FACE('',(#948,#561),#692,.T.);
#6174=ADVANCED_FACE('',(#949),#6020,.F.);
#6175=ADVANCED_FACE('',(#950),#6021,.T.);
#6176=ADVANCED_FACE('',(#951,#562,#563,#564,#565,#566),#693,.T.);
#6177=ADVANCED_FACE('',(#952,#567,#568,#569,#570,#571),#694,.F.);
#6178=ADVANCED_FACE('',(#953),#6022,.F.);
#6179=ADVANCED_FACE('',(#954),#6023,.F.);
#6180=ADVANCED_FACE('',(#955),#6024,.F.);
#6181=ADVANCED_FACE('',(#956),#6025,.F.);
#6182=ADVANCED_FACE('',(#957),#6026,.T.);
#6183=ADVANCED_FACE('',(#958,#572),#695,.F.);
#6184=ADVANCED_FACE('',(#959),#6027,.F.);
#6185=ADVANCED_FACE('',(#960),#6028,.T.);
#6186=ADVANCED_FACE('',(#961,#573,#574,#575,#576,#577),#696,.T.);
#6187=ADVANCED_FACE('',(#962,#578,#579,#580,#581,#582),#697,.F.);
#6188=ADVANCED_FACE('',(#963),#698,.T.);
#6189=ADVANCED_FACE('',(#964),#699,.T.);
#6190=ADVANCED_FACE('',(#965),#700,.T.);
#6191=ADVANCED_FACE('',(#966),#701,.T.);
#6192=ADVANCED_FACE('',(#967),#702,.T.);
#6193=ADVANCED_FACE('',(#968),#703,.F.);
#6194=ADVANCED_FACE('',(#969),#704,.T.);
#6195=ADVANCED_FACE('',(#970),#705,.T.);
#6196=ADVANCED_FACE('',(#971),#706,.T.);
#6197=ADVANCED_FACE('',(#972),#707,.T.);
#6198=ADVANCED_FACE('',(#973),#708,.T.);
#6199=ADVANCED_FACE('',(#974),#709,.F.);
#6200=ADVANCED_FACE('',(#975),#348,.F.);
#6201=ADVANCED_FACE('',(#976),#6029,.T.);
#6202=ADVANCED_FACE('',(#977),#6030,.F.);
#6203=ADVANCED_FACE('',(#978),#327,.F.);
#6204=ADVANCED_FACE('',(#979,#583),#710,.T.);
#6205=ADVANCED_FACE('',(#980),#6031,.T.);
#6206=ADVANCED_FACE('',(#981,#584),#711,.T.);
#6207=ADVANCED_FACE('',(#982),#328,.F.);
#6208=ADVANCED_FACE('',(#983),#349,.F.);
#6209=ADVANCED_FACE('',(#984),#6032,.F.);
#6210=ADVANCED_FACE('',(#985,#585),#712,.T.);
#6211=ADVANCED_FACE('',(#986),#329,.T.);
#6212=ADVANCED_FACE('',(#987),#6033,.T.);
#6213=ADVANCED_FACE('',(#988),#330,.T.);
#6214=ADVANCED_FACE('',(#989,#586),#713,.T.);
#6215=ADVANCED_FACE('',(#990),#6034,.F.);
#6216=ADVANCED_FACE('',(#991),#293,.T.);
#6217=ADVANCED_FACE('',(#992),#294,.T.);
#6218=ADVANCED_FACE('',(#993),#295,.T.);
#6219=ADVANCED_FACE('',(#994),#296,.T.);
#6220=ADVANCED_FACE('',(#995),#297,.T.);
#6221=ADVANCED_FACE('',(#996),#298,.T.);
#6222=ADVANCED_FACE('',(#997),#299,.T.);
#6223=ADVANCED_FACE('',(#998),#300,.T.);
#6224=ADVANCED_FACE('',(#999),#301,.T.);
#6225=ADVANCED_FACE('',(#1000),#302,.F.);
#6226=ADVANCED_FACE('',(#1001),#6035,.T.);
#6227=ADVANCED_FACE('',(#1002),#714,.T.);
#6228=ADVANCED_FACE('',(#1003),#303,.F.);
#6229=ADVANCED_FACE('',(#1004),#715,.T.);
#6230=ADVANCED_FACE('',(#1005),#304,.F.);
#6231=ADVANCED_FACE('',(#1006),#716,.T.);
#6232=ADVANCED_FACE('',(#1007),#305,.F.);
#6233=ADVANCED_FACE('',(#1008),#717,.T.);
#6234=ADVANCED_FACE('',(#1009),#306,.F.);
#6235=ADVANCED_FACE('',(#1010),#718,.T.);
#6236=ADVANCED_FACE('',(#1011),#307,.F.);
#6237=ADVANCED_FACE('',(#1012),#719,.T.);
#6238=ADVANCED_FACE('',(#1013),#308,.F.);
#6239=ADVANCED_FACE('',(#1014),#720,.T.);
#6240=ADVANCED_FACE('',(#1015),#309,.F.);
#6241=ADVANCED_FACE('',(#1016),#6036,.F.);
#6242=ADVANCED_FACE('',(#1017),#721,.T.);
#6243=ADVANCED_FACE('',(#1018),#310,.F.);
#6244=ADVANCED_FACE('',(#1019,#587),#722,.T.);
#6245=ADVANCED_FACE('',(#1020),#723,.T.);
#6246=ADVANCED_FACE('',(#1021,#588),#724,.T.);
#6247=ADVANCED_FACE('',(#1022),#6037,.T.);
#6248=ADVANCED_FACE('',(#1023,#589),#725,.T.);
#6249=ADVANCED_FACE('',(#1024),#6038,.F.);
#6250=ADVANCED_FACE('',(#1025,#590),#726,.T.);
#6251=ADVANCED_FACE('',(#1026),#6039,.T.);
#6252=ADVANCED_FACE('',(#1027,#591),#727,.T.);
#6253=ADVANCED_FACE('',(#1028),#6040,.F.);
#6254=ADVANCED_FACE('',(#1029),#728,.T.);
#6255=ADVANCED_FACE('',(#1030),#331,.T.);
#6256=ADVANCED_FACE('',(#1031),#6041,.T.);
#6257=ADVANCED_FACE('',(#1032),#332,.T.);
#6258=ADVANCED_FACE('',(#1033,#592),#729,.T.);
#6259=ADVANCED_FACE('',(#1034),#333,.T.);
#6260=ADVANCED_FACE('',(#1035),#6042,.T.);
#6261=ADVANCED_FACE('',(#1036),#334,.T.);
#6262=ADVANCED_FACE('',(#1037),#730,.T.);
#6263=ADVANCED_FACE('',(#1038),#731,.F.);
#6264=ADVANCED_FACE('',(#1039),#732,.F.);
#6265=ADVANCED_FACE('',(#1040),#733,.F.);
#6266=ADVANCED_FACE('',(#1041),#734,.F.);
#6267=ADVANCED_FACE('',(#1042),#735,.F.);
#6268=ADVANCED_FACE('',(#1043),#736,.F.);
#6269=ADVANCED_FACE('',(#1044),#737,.F.);
#6270=ADVANCED_FACE('',(#1045),#738,.F.);
#6271=ADVANCED_FACE('',(#1046),#739,.T.);
#6272=ADVANCED_FACE('',(#1047),#335,.T.);
#6273=ADVANCED_FACE('',(#1048),#6043,.T.);
#6274=ADVANCED_FACE('',(#1049),#336,.T.);
#6275=ADVANCED_FACE('',(#1050,#593),#740,.T.);
#6276=ADVANCED_FACE('',(#1051),#337,.T.);
#6277=ADVANCED_FACE('',(#1052),#6044,.T.);
#6278=ADVANCED_FACE('',(#1053),#338,.T.);
#6279=ADVANCED_FACE('',(#1054),#741,.T.);
#6280=ADVANCED_FACE('',(#1055),#742,.F.);
#6281=ADVANCED_FACE('',(#1056),#743,.F.);
#6282=ADVANCED_FACE('',(#1057),#744,.F.);
#6283=ADVANCED_FACE('',(#1058),#745,.F.);
#6284=ADVANCED_FACE('',(#1059),#746,.F.);
#6285=ADVANCED_FACE('',(#1060),#747,.F.);
#6286=ADVANCED_FACE('',(#1061),#748,.F.);
#6287=ADVANCED_FACE('',(#1062),#749,.F.);
#6288=ADVANCED_FACE('',(#1063),#750,.F.);
#6289=ADVANCED_FACE('',(#1064),#751,.T.);
#6290=ADVANCED_FACE('',(#1065),#752,.F.);
#6291=ADVANCED_FACE('',(#1066),#753,.F.);
#6292=ADVANCED_FACE('',(#1067),#754,.F.);
#6293=ADVANCED_FACE('',(#1068),#755,.F.);
#6294=ADVANCED_FACE('',(#1069),#756,.T.);
#6295=ADVANCED_FACE('',(#1070),#757,.F.);
#6296=ADVANCED_FACE('',(#1071),#758,.F.);
#6297=ADVANCED_FACE('',(#1072),#759,.F.);
#6298=ADVANCED_FACE('',(#1073,#594),#760,.T.);
#6299=ADVANCED_FACE('',(#1074,#595),#761,.F.);
#6300=ADVANCED_FACE('',(#1075),#6045,.T.);
#6301=ADVANCED_FACE('',(#1076,#596),#6046,.T.);
#6302=ADVANCED_FACE('',(#1077,#597),#6047,.T.);
#6303=ADVANCED_FACE('',(#1078),#762,.T.);
#6304=ADVANCED_FACE('',(#1079),#763,.F.);
#6305=ADVANCED_FACE('',(#1080),#6048,.F.);
#6306=ADVANCED_FACE('',(#1081),#6049,.T.);
#6307=ADVANCED_FACE('',(#1082,#598),#764,.T.);
#6308=ADVANCED_FACE('',(#1083,#599),#765,.F.);
#6309=ADVANCED_FACE('',(#1084),#766,.T.);
#6310=ADVANCED_FACE('',(#1085),#6050,.F.);
#6311=ADVANCED_FACE('',(#1086),#767,.T.);
#6312=ADVANCED_FACE('',(#1087,#600),#6051,.F.);
#6313=ADVANCED_FACE('',(#1088,#601),#6052,.T.);
#6314=ADVANCED_FACE('',(#1089,#602),#768,.T.);
#6315=ADVANCED_FACE('',(#1090,#603),#769,.F.);
#6316=ADVANCED_FACE('',(#1091),#770,.T.);
#6317=ADVANCED_FACE('',(#1092),#6053,.F.);
#6318=ADVANCED_FACE('',(#1093),#771,.T.);
#6319=ADVANCED_FACE('',(#1094),#772,.F.);
#6320=ADVANCED_FACE('',(#1095),#773,.F.);
#6321=ADVANCED_FACE('',(#1096),#774,.F.);
#6322=ADVANCED_FACE('',(#1097),#775,.F.);
#6323=ADVANCED_FACE('',(#1098),#776,.T.);
#6324=ADVANCED_FACE('',(#1099,#604),#777,.T.);
#6325=ADVANCED_FACE('',(#1100),#778,.T.);
#6326=ADVANCED_FACE('',(#1101),#779,.T.);
#6327=ADVANCED_FACE('',(#1102),#780,.T.);
#6328=ADVANCED_FACE('',(#1103),#781,.T.);
#6329=ADVANCED_FACE('',(#1104),#782,.F.);
#6330=ADVANCED_FACE('',(#1105),#783,.T.);
#6331=ADVANCED_FACE('',(#1106,#605),#784,.F.);
#6332=ADVANCED_FACE('',(#1107,#606),#6054,.F.);
#6333=ADVANCED_FACE('',(#1108,#607),#6055,.T.);
#6334=ADVANCED_FACE('',(#1109),#785,.T.);
#6335=ADVANCED_FACE('',(#1110),#6056,.F.);
#6336=ADVANCED_FACE('',(#1111),#786,.T.);
#6337=ADVANCED_FACE('',(#1112),#787,.F.);
#6338=ADVANCED_FACE('',(#1113),#788,.F.);
#6339=ADVANCED_FACE('',(#1114),#789,.F.);
#6340=ADVANCED_FACE('',(#1115,#608),#790,.T.);
#6341=ADVANCED_FACE('',(#1116,#609),#6057,.F.);
#6342=ADVANCED_FACE('',(#1117),#6058,.F.);
#6343=ADVANCED_FACE('',(#1118),#6059,.T.);
#6344=ADVANCED_FACE('',(#1119,#610),#791,.F.);
#6345=ADVANCED_FACE('',(#1120),#792,.T.);
#6346=ADVANCED_FACE('',(#1121,#611),#793,.T.);
#6347=ADVANCED_FACE('',(#1122),#794,.T.);
#6348=ADVANCED_FACE('',(#1123,#612,#613),#6060,.T.);
#6349=ADVANCED_FACE('',(#1124,#614),#795,.F.);
#6350=ADVANCED_FACE('',(#1125),#6061,.T.);
#6351=ADVANCED_FACE('',(#1126,#615),#796,.T.);
#6352=ADVANCED_FACE('',(#1127),#6062,.F.);
#6353=ADVANCED_FACE('',(#1128),#6063,.T.);
#6354=ADVANCED_FACE('',(#1129,#616),#797,.T.);
#6355=ADVANCED_FACE('',(#1130,#617),#798,.F.);
#6356=ADVANCED_FACE('',(#1131),#6064,.T.);
#6357=ADVANCED_FACE('',(#1132,#618),#799,.F.);
#6358=ADVANCED_FACE('',(#1133),#6065,.F.);
#6359=ADVANCED_FACE('',(#1134),#6066,.T.);
#6360=ADVANCED_FACE('',(#1135,#619),#800,.T.);
#6361=ADVANCED_FACE('',(#1136,#620),#801,.F.);
#6362=ADVANCED_FACE('',(#1137),#802,.T.);
#6363=ADVANCED_FACE('',(#1138),#803,.T.);
#6364=ADVANCED_FACE('',(#1139),#804,.T.);
#6365=ADVANCED_FACE('',(#1140),#805,.T.);
#6366=ADVANCED_FACE('',(#1141),#806,.T.);
#6367=ADVANCED_FACE('',(#1142),#807,.F.);
#6368=ADVANCED_FACE('',(#1143),#808,.T.);
#6369=ADVANCED_FACE('',(#1144),#809,.T.);
#6370=ADVANCED_FACE('',(#1145),#810,.T.);
#6371=ADVANCED_FACE('',(#1146),#811,.F.);
#6372=ADVANCED_FACE('',(#1147),#812,.F.);
#6373=ADVANCED_FACE('',(#1148),#813,.F.);
#6374=ADVANCED_FACE('',(#1149),#814,.F.);
#6375=ADVANCED_FACE('',(#1150),#815,.F.);
#6376=ADVANCED_FACE('',(#1151),#816,.F.);
#6377=ADVANCED_FACE('',(#1152),#817,.F.);
#6378=ADVANCED_FACE('',(#1153),#818,.F.);
#6379=ADVANCED_FACE('',(#1154,#621),#819,.T.);
#6380=ADVANCED_FACE('',(#1155),#339,.T.);
#6381=ADVANCED_FACE('',(#1156),#6067,.T.);
#6382=ADVANCED_FACE('',(#1157),#340,.T.);
#6383=ADVANCED_FACE('',(#1158),#820,.T.);
#6384=ADVANCED_FACE('',(#1159),#350,.F.);
#6385=ADVANCED_FACE('',(#1160),#6068,.T.);
#6386=ADVANCED_FACE('',(#1161),#6069,.F.);
#6387=ADVANCED_FACE('',(#1162),#341,.F.);
#6388=ADVANCED_FACE('',(#1163,#622),#821,.T.);
#6389=ADVANCED_FACE('',(#1164),#6070,.T.);
#6390=ADVANCED_FACE('',(#1165,#623),#822,.T.);
#6391=ADVANCED_FACE('',(#1166),#342,.F.);
#6392=ADVANCED_FACE('',(#1167),#351,.F.);
#6393=ADVANCED_FACE('',(#1168),#6071,.F.);
#6394=ADVANCED_FACE('',(#1169,#624),#823,.T.);
#6395=ADVANCED_FACE('',(#1170),#343,.T.);
#6396=ADVANCED_FACE('',(#1171),#6072,.T.);
#6397=ADVANCED_FACE('',(#1172),#344,.T.);
#6398=ADVANCED_FACE('',(#1173,#625),#824,.T.);
#6399=ADVANCED_FACE('',(#1174),#6073,.F.);
#6400=ADVANCED_FACE('',(#1175),#311,.T.);
#6401=ADVANCED_FACE('',(#1176),#312,.T.);
#6402=ADVANCED_FACE('',(#1177),#313,.T.);
#6403=ADVANCED_FACE('',(#1178),#314,.T.);
#6404=ADVANCED_FACE('',(#1179),#315,.T.);
#6405=ADVANCED_FACE('',(#1180),#316,.T.);
#6406=ADVANCED_FACE('',(#1181),#317,.T.);
#6407=ADVANCED_FACE('',(#1182),#318,.T.);
#6408=ADVANCED_FACE('',(#1183),#319,.F.);
#6409=ADVANCED_FACE('',(#1184),#6074,.T.);
#6410=ADVANCED_FACE('',(#1185),#825,.T.);
#6411=ADVANCED_FACE('',(#1186),#320,.F.);
#6412=ADVANCED_FACE('',(#1187),#826,.T.);
#6413=ADVANCED_FACE('',(#1188),#321,.F.);
#6414=ADVANCED_FACE('',(#1189),#827,.T.);
#6415=ADVANCED_FACE('',(#1190),#322,.F.);
#6416=ADVANCED_FACE('',(#1191),#828,.T.);
#6417=ADVANCED_FACE('',(#1192),#323,.F.);
#6418=ADVANCED_FACE('',(#1193),#829,.T.);
#6419=ADVANCED_FACE('',(#1194),#324,.F.);
#6420=ADVANCED_FACE('',(#1195),#830,.T.);
#6421=ADVANCED_FACE('',(#1196),#325,.F.);
#6422=ADVANCED_FACE('',(#1197),#6075,.F.);
#6423=ADVANCED_FACE('',(#1198),#831,.T.);
#6424=ADVANCED_FACE('',(#1199),#326,.F.);
#6425=ADVANCED_FACE('',(#1200,#626),#832,.T.);
#6426=ADVANCED_FACE('',(#1201),#833,.T.);
#6427=ADVANCED_FACE('',(#1202,#627),#834,.T.);
#6428=ADVANCED_FACE('',(#1203),#6076,.T.);
#6429=ADVANCED_FACE('',(#1204,#628),#835,.T.);
#6430=ADVANCED_FACE('',(#1205),#6077,.F.);
#6431=ADVANCED_FACE('',(#1206,#629),#836,.T.);
#6432=ADVANCED_FACE('',(#1207),#6078,.T.);
#6433=ADVANCED_FACE('',(#1208,#630),#837,.T.);
#6434=ADVANCED_FACE('',(#1209),#6079,.F.);
#6435=ADVANCED_FACE('',(#1210),#6080,.F.);
#6436=ADVANCED_FACE('',(#1211),#6081,.F.);
#6437=ADVANCED_FACE('',(#1212),#6082,.F.);
#6438=ADVANCED_FACE('',(#1213,#631),#838,.T.);
#6439=ADVANCED_FACE('',(#1214),#839,.T.);
#6440=ADVANCED_FACE('',(#1215,#632),#840,.T.);
#6441=ADVANCED_FACE('',(#1216,#633),#841,.F.);
#6442=ADVANCED_FACE('',(#1217,#634),#842,.T.);
#6443=ADVANCED_FACE('',(#1218),#843,.T.);
#6444=ADVANCED_FACE('',(#1219,#635),#844,.T.);
#6445=ADVANCED_FACE('',(#1220),#845,.T.);
#6446=ADVANCED_FACE('',(#1221),#846,.T.);
#6447=ADVANCED_FACE('',(#1222,#636),#847,.F.);
#6448=ADVANCED_FACE('',(#1223),#6083,.F.);
#6449=ADVANCED_FACE('',(#1224),#848,.T.);
#6450=ADVANCED_FACE('',(#1225),#6084,.F.);
#6451=ADVANCED_FACE('',(#1226),#849,.F.);
#6452=ADVANCED_FACE('',(#1227),#6085,.T.);
#6453=ADVANCED_FACE('',(#1228,#637),#850,.T.);
#6454=ADVANCED_FACE('',(#1229,#638),#851,.F.);
#6455=ADVANCED_FACE('',(#1230),#6086,.F.);
#6456=ADVANCED_FACE('',(#1231),#6087,.T.);
#6457=ADVANCED_FACE('',(#1232,#639),#852,.T.);
#6458=ADVANCED_FACE('',(#1233,#640),#853,.F.);
#6459=ADVANCED_FACE('',(#1234),#6088,.F.);
#6460=ADVANCED_FACE('',(#1235),#6089,.T.);
#6461=ADVANCED_FACE('',(#1236,#641),#854,.T.);
#6462=ADVANCED_FACE('',(#1237,#642),#855,.F.);
#6463=ADVANCED_FACE('',(#1238),#6090,.F.);
#6464=ADVANCED_FACE('',(#1239),#6091,.T.);
#6465=ADVANCED_FACE('',(#1240,#643),#856,.T.);
#6466=ADVANCED_FACE('',(#1241,#644),#857,.F.);
#6467=ADVANCED_FACE('',(#1242),#6092,.F.);
#6468=ADVANCED_FACE('',(#1243),#6093,.T.);
#6469=ADVANCED_FACE('',(#1244,#645),#858,.T.);
#6470=ADVANCED_FACE('',(#1245,#646),#859,.F.);
#6471=ADVANCED_FACE('',(#1246),#6094,.F.);
#6472=ADVANCED_FACE('',(#1247),#6095,.T.);
#6473=ADVANCED_FACE('',(#1248,#647),#860,.T.);
#6474=ADVANCED_FACE('',(#1249,#648),#861,.F.);
#6475=ADVANCED_FACE('',(#1250),#6096,.F.);
#6476=ADVANCED_FACE('',(#1251),#6097,.T.);
#6477=ADVANCED_FACE('',(#1252,#649),#862,.T.);
#6478=ADVANCED_FACE('',(#1253,#650),#863,.F.);
#6479=ADVANCED_FACE('',(#1254),#864,.F.);
#6480=ADVANCED_FACE('',(#1255),#865,.F.);
#6481=ADVANCED_FACE('',(#1256),#866,.F.);
#6482=ADVANCED_FACE('',(#1257),#867,.F.);
#6483=ADVANCED_FACE('',(#1258),#868,.F.);
#6484=ADVANCED_FACE('',(#1259),#869,.F.);
#6485=ADVANCED_FACE('',(#1260),#870,.F.);
#6486=ADVANCED_FACE('',(#1261),#871,.F.);
#6487=ADVANCED_FACE('',(#1262),#872,.F.);
#6488=ADVANCED_FACE('',(#1263),#873,.T.);
#6489=ADVANCED_FACE('',(#1264),#345,.T.);
#6490=ADVANCED_FACE('',(#1265),#6098,.T.);
#6491=ADVANCED_FACE('',(#1266),#346,.T.);
#6492=ADVANCED_FACE('',(#1267,#651),#874,.T.);
#6493=ADVANCED_FACE('',(#1268),#347,.T.);
#6494=ADVANCED_FACE('',(#1269),#6099,.T.);
#6495=CLOSED_SHELL('',(#6100,#6101,#6102,#6103,#6104,#6105,#6106,#6107,
#6108,#6109));
#6496=CLOSED_SHELL('',(#6110,#6111,#6112,#6113,#6114,#6115,#6116,#6117,
#6118,#6119,#6120,#6121,#6122,#6123,#6124,#6125,#6126,#6127,#6128,#6129,
#6130,#6131,#6132,#6133,#6134,#6135,#6136,#6137,#6138,#6139,#6140,#6141,
#6142,#6143,#6144,#6145,#6146,#6147,#6148,#6149,#6150,#6151,#6152,#6153,
#6154,#6155,#6156,#6157,#6158,#6159,#6160,#6161,#6162,#6163));
#6497=CLOSED_SHELL('',(#6164,#6165,#6166,#6167));
#6498=CLOSED_SHELL('',(#6168,#6169,#6170,#6171,#6172,#6173,#6174,#6175,
#6176,#6177));
#6499=CLOSED_SHELL('',(#6178,#6179,#6180,#6181,#6182,#6183,#6184,#6185,
#6186,#6187));
#6500=CLOSED_SHELL('',(#6188,#6189,#6190,#6191,#6192,#6193));
#6501=CLOSED_SHELL('',(#6194,#6195,#6196,#6197,#6198,#6199));
#6502=CLOSED_SHELL('',(#6200,#6201,#6202,#6203,#6204,#6205,#6206,#6207));
#6503=CLOSED_SHELL('',(#6208,#6209,#6210,#6211,#6212,#6213,#6214,#6215));
#6504=CLOSED_SHELL('',(#6216));
#6505=CLOSED_SHELL('',(#6217));
#6506=CLOSED_SHELL('',(#6218));
#6507=CLOSED_SHELL('',(#6219));
#6508=CLOSED_SHELL('',(#6220));
#6509=CLOSED_SHELL('',(#6221));
#6510=CLOSED_SHELL('',(#6222));
#6511=CLOSED_SHELL('',(#6223));
#6512=CLOSED_SHELL('',(#6224));
#6513=CLOSED_SHELL('',(#6225,#6226,#6227,#6228,#6229,#6230,#6231,#6232,
#6233,#6234,#6235,#6236,#6237,#6238,#6239,#6240,#6241,#6242,#6243,#6244,
#6245));
#6514=CLOSED_SHELL('',(#6246,#6247,#6248,#6249));
#6515=CLOSED_SHELL('',(#6250,#6251,#6252,#6253));
#6516=CLOSED_SHELL('',(#6254,#6255,#6256,#6257,#6258,#6259,#6260,#6261,
#6262));
#6517=CLOSED_SHELL('',(#6263,#6264,#6265,#6266,#6267,#6268,#6269,#6270));
#6518=CLOSED_SHELL('',(#6271,#6272,#6273,#6274,#6275,#6276,#6277,#6278,
#6279));
#6519=CLOSED_SHELL('',(#6280,#6281,#6282,#6283,#6284,#6285,#6286,#6287));
#6520=CLOSED_SHELL('',(#6288,#6289,#6290,#6291,#6292,#6293,#6294,#6295,
#6296,#6297,#6298,#6299,#6300,#6301,#6302,#6303,#6304));
#6521=CLOSED_SHELL('',(#6305,#6306,#6307,#6308));
#6522=CLOSED_SHELL('',(#6309,#6310,#6311,#6312,#6313,#6314,#6315));
#6523=CLOSED_SHELL('',(#6316,#6317,#6318,#6319,#6320,#6321,#6322,#6323,
#6324,#6325,#6326,#6327,#6328,#6329,#6330,#6331,#6332,#6333));
#6524=CLOSED_SHELL('',(#6334,#6335,#6336,#6337,#6338,#6339,#6340,#6341,
#6342,#6343,#6344,#6345,#6346,#6347,#6348,#6349));
#6525=CLOSED_SHELL('',(#6350,#6351,#6352,#6353,#6354,#6355));
#6526=CLOSED_SHELL('',(#6356,#6357,#6358,#6359,#6360,#6361));
#6527=CLOSED_SHELL('',(#6362,#6363,#6364,#6365,#6366,#6367,#6368,#6369,
#6370,#6371));
#6528=CLOSED_SHELL('',(#6372,#6373,#6374,#6375,#6376,#6377,#6378,#6379,
#6380,#6381,#6382,#6383));
#6529=CLOSED_SHELL('',(#6384,#6385,#6386,#6387,#6388,#6389,#6390,#6391));
#6530=CLOSED_SHELL('',(#6392,#6393,#6394,#6395,#6396,#6397,#6398,#6399));
#6531=CLOSED_SHELL('',(#6400));
#6532=CLOSED_SHELL('',(#6401));
#6533=CLOSED_SHELL('',(#6402));
#6534=CLOSED_SHELL('',(#6403));
#6535=CLOSED_SHELL('',(#6404));
#6536=CLOSED_SHELL('',(#6405));
#6537=CLOSED_SHELL('',(#6406));
#6538=CLOSED_SHELL('',(#6407));
#6539=CLOSED_SHELL('',(#6408,#6409,#6410,#6411,#6412,#6413,#6414,#6415,
#6416,#6417,#6418,#6419,#6420,#6421,#6422,#6423,#6424,#6425,#6426));
#6540=CLOSED_SHELL('',(#6427,#6428,#6429,#6430));
#6541=CLOSED_SHELL('',(#6431,#6432,#6433,#6434));
#6542=CLOSED_SHELL('',(#6435,#6436,#6437,#6438,#6439,#6440,#6441,#6442,
#6443,#6444,#6445,#6446,#6447));
#6543=CLOSED_SHELL('',(#6448,#6449,#6450,#6451,#6452,#6453,#6454));
#6544=CLOSED_SHELL('',(#6455,#6456,#6457,#6458));
#6545=CLOSED_SHELL('',(#6459,#6460,#6461,#6462));
#6546=CLOSED_SHELL('',(#6463,#6464,#6465,#6466));
#6547=CLOSED_SHELL('',(#6467,#6468,#6469,#6470));
#6548=CLOSED_SHELL('',(#6471,#6472,#6473,#6474));
#6549=CLOSED_SHELL('',(#6475,#6476,#6477,#6478));
#6550=CLOSED_SHELL('',(#6479,#6480,#6481,#6482,#6483,#6484,#6485,#6486));
#6551=CLOSED_SHELL('',(#6487,#6488,#6489,#6490,#6491,#6492,#6493,#6494));
#6552=DERIVED_UNIT_ELEMENT(#6626,1.);
#6553=DERIVED_UNIT_ELEMENT(#12785,-3.);
#6554=DERIVED_UNIT_ELEMENT(#6626,1.);
#6555=DERIVED_UNIT_ELEMENT(#12785,-3.);
#6556=DERIVED_UNIT_ELEMENT(#6626,1.);
#6557=DERIVED_UNIT_ELEMENT(#12785,-3.);
#6558=DERIVED_UNIT_ELEMENT(#6626,1.);
#6559=DERIVED_UNIT_ELEMENT(#12785,-3.);
#6560=DERIVED_UNIT_ELEMENT(#6626,1.);
#6561=DERIVED_UNIT_ELEMENT(#12785,-3.);
#6562=DERIVED_UNIT_ELEMENT(#6626,1.);
#6563=DERIVED_UNIT_ELEMENT(#12785,-3.);
#6564=DERIVED_UNIT_ELEMENT(#6626,1.);
#6565=DERIVED_UNIT_ELEMENT(#12785,-3.);
#6566=DERIVED_UNIT_ELEMENT(#6626,1.);
#6567=DERIVED_UNIT_ELEMENT(#12785,-3.);
#6568=DERIVED_UNIT_ELEMENT(#6626,1.);
#6569=DERIVED_UNIT_ELEMENT(#12785,-3.);
#6570=DERIVED_UNIT_ELEMENT(#6626,1.);
#6571=DERIVED_UNIT_ELEMENT(#12785,-3.);
#6572=DERIVED_UNIT_ELEMENT(#6626,1.);
#6573=DERIVED_UNIT_ELEMENT(#12785,-3.);
#6574=DERIVED_UNIT_ELEMENT(#6626,1.);
#6575=DERIVED_UNIT_ELEMENT(#12785,-3.);
#6576=DERIVED_UNIT_ELEMENT(#6626,1.);
#6577=DERIVED_UNIT_ELEMENT(#12785,-3.);
#6578=DERIVED_UNIT_ELEMENT(#6626,1.);
#6579=DERIVED_UNIT_ELEMENT(#12785,-3.);
#6580=DERIVED_UNIT_ELEMENT(#6626,1.);
#6581=DERIVED_UNIT_ELEMENT(#12785,-3.);
#6582=DERIVED_UNIT_ELEMENT(#6626,1.);
#6583=DERIVED_UNIT_ELEMENT(#12785,-3.);
#6584=DERIVED_UNIT_ELEMENT(#6626,1.);
#6585=DERIVED_UNIT_ELEMENT(#12785,-3.);
#6586=DERIVED_UNIT_ELEMENT(#6626,1.);
#6587=DERIVED_UNIT_ELEMENT(#12785,-3.);
#6588=DERIVED_UNIT_ELEMENT(#6626,1.);
#6589=DERIVED_UNIT_ELEMENT(#12785,-3.);
#6590=DERIVED_UNIT_ELEMENT(#6626,1.);
#6591=DERIVED_UNIT_ELEMENT(#12785,-3.);
#6592=DERIVED_UNIT_ELEMENT(#6626,1.);
#6593=DERIVED_UNIT_ELEMENT(#12785,-3.);
#6594=DERIVED_UNIT_ELEMENT(#6626,1.);
#6595=DERIVED_UNIT_ELEMENT(#12785,-3.);
#6596=DERIVED_UNIT_ELEMENT(#6626,1.);
#6597=DERIVED_UNIT_ELEMENT(#12785,-3.);
#6598=DERIVED_UNIT_ELEMENT(#6626,1.);
#6599=DERIVED_UNIT_ELEMENT(#12785,-3.);
#6600=DERIVED_UNIT_ELEMENT(#6626,1.);
#6601=DERIVED_UNIT_ELEMENT(#12785,-3.);
#6602=DERIVED_UNIT_ELEMENT(#6626,1.);
#6603=DERIVED_UNIT_ELEMENT(#12785,-3.);
#6604=DERIVED_UNIT_ELEMENT(#6626,1.);
#6605=DERIVED_UNIT_ELEMENT(#12785,-3.);
#6606=DERIVED_UNIT_ELEMENT(#6626,1.);
#6607=DERIVED_UNIT_ELEMENT(#12785,-3.);
#6608=DERIVED_UNIT_ELEMENT(#6626,1.);
#6609=DERIVED_UNIT_ELEMENT(#12785,-3.);
#6610=DERIVED_UNIT_ELEMENT(#6626,1.);
#6611=DERIVED_UNIT_ELEMENT(#12785,-3.);
#6612=DERIVED_UNIT_ELEMENT(#6626,1.);
#6613=DERIVED_UNIT_ELEMENT(#12785,-3.);
#6614=DERIVED_UNIT_ELEMENT(#6626,1.);
#6615=DERIVED_UNIT_ELEMENT(#12785,-3.);
#6616=DERIVED_UNIT_ELEMENT(#6626,1.);
#6617=DERIVED_UNIT_ELEMENT(#12785,-3.);
#6618=DERIVED_UNIT_ELEMENT(#6626,1.);
#6619=DERIVED_UNIT_ELEMENT(#12785,-3.);
#6620=DERIVED_UNIT_ELEMENT(#6626,1.);
#6621=DERIVED_UNIT_ELEMENT(#12785,-3.);
#6622=DERIVED_UNIT_ELEMENT(#6626,1.);
#6623=DERIVED_UNIT_ELEMENT(#12785,-3.);
#6624=DERIVED_UNIT_ELEMENT(#6626,1.);
#6625=DERIVED_UNIT_ELEMENT(#12785,-3.);
#6626=(
MASS_UNIT()
NAMED_UNIT(*)
SI_UNIT(.KILO.,.GRAM.)
);
#6627=DERIVED_UNIT((#6552,#6553));
#6628=DERIVED_UNIT((#6554,#6555));
#6629=DERIVED_UNIT((#6556,#6557));
#6630=DERIVED_UNIT((#6558,#6559));
#6631=DERIVED_UNIT((#6560,#6561));
#6632=DERIVED_UNIT((#6562,#6563));
#6633=DERIVED_UNIT((#6564,#6565));
#6634=DERIVED_UNIT((#6566,#6567));
#6635=DERIVED_UNIT((#6568,#6569));
#6636=DERIVED_UNIT((#6570,#6571));
#6637=DERIVED_UNIT((#6572,#6573));
#6638=DERIVED_UNIT((#6574,#6575));
#6639=DERIVED_UNIT((#6576,#6577));
#6640=DERIVED_UNIT((#6578,#6579));
#6641=DERIVED_UNIT((#6580,#6581));
#6642=DERIVED_UNIT((#6582,#6583));
#6643=DERIVED_UNIT((#6584,#6585));
#6644=DERIVED_UNIT((#6586,#6587));
#6645=DERIVED_UNIT((#6588,#6589));
#6646=DERIVED_UNIT((#6590,#6591));
#6647=DERIVED_UNIT((#6592,#6593));
#6648=DERIVED_UNIT((#6594,#6595));
#6649=DERIVED_UNIT((#6596,#6597));
#6650=DERIVED_UNIT((#6598,#6599));
#6651=DERIVED_UNIT((#6600,#6601));
#6652=DERIVED_UNIT((#6602,#6603));
#6653=DERIVED_UNIT((#6604,#6605));
#6654=DERIVED_UNIT((#6606,#6607));
#6655=DERIVED_UNIT((#6608,#6609));
#6656=DERIVED_UNIT((#6610,#6611));
#6657=DERIVED_UNIT((#6612,#6613));
#6658=DERIVED_UNIT((#6614,#6615));
#6659=DERIVED_UNIT((#6616,#6617));
#6660=DERIVED_UNIT((#6618,#6619));
#6661=DERIVED_UNIT((#6620,#6621));
#6662=DERIVED_UNIT((#6622,#6623));
#6663=DERIVED_UNIT((#6624,#6625));
#6664=MEASURE_REPRESENTATION_ITEM('density measure',
POSITIVE_RATIO_MEASURE(7850.),#6627);
#6665=MEASURE_REPRESENTATION_ITEM('density measure',
POSITIVE_RATIO_MEASURE(7850.),#6628);
#6666=MEASURE_REPRESENTATION_ITEM('density measure',
POSITIVE_RATIO_MEASURE(7850.),#6629);
#6667=MEASURE_REPRESENTATION_ITEM('density measure',
POSITIVE_RATIO_MEASURE(7850.),#6630);
#6668=MEASURE_REPRESENTATION_ITEM('density measure',
POSITIVE_RATIO_MEASURE(7850.),#6631);
#6669=MEASURE_REPRESENTATION_ITEM('density measure',
POSITIVE_RATIO_MEASURE(7850.),#6632);
#6670=MEASURE_REPRESENTATION_ITEM('density measure',
POSITIVE_RATIO_MEASURE(7850.),#6633);
#6671=MEASURE_REPRESENTATION_ITEM('density measure',
POSITIVE_RATIO_MEASURE(7850.),#6634);
#6672=MEASURE_REPRESENTATION_ITEM('density measure',
POSITIVE_RATIO_MEASURE(7850.),#6635);
#6673=MEASURE_REPRESENTATION_ITEM('density measure',
POSITIVE_RATIO_MEASURE(7850.),#6636);
#6674=MEASURE_REPRESENTATION_ITEM('density measure',
POSITIVE_RATIO_MEASURE(7850.),#6637);
#6675=MEASURE_REPRESENTATION_ITEM('density measure',
POSITIVE_RATIO_MEASURE(7850.),#6638);
#6676=MEASURE_REPRESENTATION_ITEM('density measure',
POSITIVE_RATIO_MEASURE(7850.),#6639);
#6677=MEASURE_REPRESENTATION_ITEM('density measure',
POSITIVE_RATIO_MEASURE(7850.),#6640);
#6678=MEASURE_REPRESENTATION_ITEM('density measure',
POSITIVE_RATIO_MEASURE(7850.),#6641);
#6679=MEASURE_REPRESENTATION_ITEM('density measure',
POSITIVE_RATIO_MEASURE(7850.),#6642);
#6680=MEASURE_REPRESENTATION_ITEM('density measure',
POSITIVE_RATIO_MEASURE(7850.),#6643);
#6681=MEASURE_REPRESENTATION_ITEM('density measure',
POSITIVE_RATIO_MEASURE(7850.),#6644);
#6682=MEASURE_REPRESENTATION_ITEM('density measure',
POSITIVE_RATIO_MEASURE(7850.),#6645);
#6683=MEASURE_REPRESENTATION_ITEM('density measure',
POSITIVE_RATIO_MEASURE(7850.),#6646);
#6684=MEASURE_REPRESENTATION_ITEM('density measure',
POSITIVE_RATIO_MEASURE(7850.),#6647);
#6685=MEASURE_REPRESENTATION_ITEM('density measure',
POSITIVE_RATIO_MEASURE(7850.),#6648);
#6686=MEASURE_REPRESENTATION_ITEM('density measure',
POSITIVE_RATIO_MEASURE(7850.),#6649);
#6687=MEASURE_REPRESENTATION_ITEM('density measure',
POSITIVE_RATIO_MEASURE(7850.),#6650);
#6688=MEASURE_REPRESENTATION_ITEM('density measure',
POSITIVE_RATIO_MEASURE(7850.),#6651);
#6689=MEASURE_REPRESENTATION_ITEM('density measure',
POSITIVE_RATIO_MEASURE(7850.),#6652);
#6690=MEASURE_REPRESENTATION_ITEM('density measure',
POSITIVE_RATIO_MEASURE(7850.),#6653);
#6691=MEASURE_REPRESENTATION_ITEM('density measure',
POSITIVE_RATIO_MEASURE(7850.),#6654);
#6692=MEASURE_REPRESENTATION_ITEM('density measure',
POSITIVE_RATIO_MEASURE(7850.),#6655);
#6693=MEASURE_REPRESENTATION_ITEM('density measure',
POSITIVE_RATIO_MEASURE(7850.),#6656);
#6694=MEASURE_REPRESENTATION_ITEM('density measure',
POSITIVE_RATIO_MEASURE(7850.),#6657);
#6695=MEASURE_REPRESENTATION_ITEM('density measure',
POSITIVE_RATIO_MEASURE(7850.),#6658);
#6696=MEASURE_REPRESENTATION_ITEM('density measure',
POSITIVE_RATIO_MEASURE(7850.),#6659);
#6697=MEASURE_REPRESENTATION_ITEM('density measure',
POSITIVE_RATIO_MEASURE(7850.),#6660);
#6698=MEASURE_REPRESENTATION_ITEM('density measure',
POSITIVE_RATIO_MEASURE(7850.),#6661);
#6699=MEASURE_REPRESENTATION_ITEM('density measure',
POSITIVE_RATIO_MEASURE(7850.),#6662);
#6700=MEASURE_REPRESENTATION_ITEM('density measure',
POSITIVE_RATIO_MEASURE(7850.),#6663);
#6701=PROPERTY_DEFINITION_REPRESENTATION(#6886,#6775);
#6702=PROPERTY_DEFINITION_REPRESENTATION(#6887,#6776);
#6703=PROPERTY_DEFINITION_REPRESENTATION(#6888,#6777);
#6704=PROPERTY_DEFINITION_REPRESENTATION(#6889,#6778);
#6705=PROPERTY_DEFINITION_REPRESENTATION(#6890,#6779);
#6706=PROPERTY_DEFINITION_REPRESENTATION(#6891,#6780);
#6707=PROPERTY_DEFINITION_REPRESENTATION(#6892,#6781);
#6708=PROPERTY_DEFINITION_REPRESENTATION(#6893,#6782);
#6709=PROPERTY_DEFINITION_REPRESENTATION(#6894,#6783);
#6710=PROPERTY_DEFINITION_REPRESENTATION(#6895,#6784);
#6711=PROPERTY_DEFINITION_REPRESENTATION(#6896,#6785);
#6712=PROPERTY_DEFINITION_REPRESENTATION(#6897,#6786);
#6713=PROPERTY_DEFINITION_REPRESENTATION(#6898,#6787);
#6714=PROPERTY_DEFINITION_REPRESENTATION(#6899,#6788);
#6715=PROPERTY_DEFINITION_REPRESENTATION(#6900,#6789);
#6716=PROPERTY_DEFINITION_REPRESENTATION(#6901,#6790);
#6717=PROPERTY_DEFINITION_REPRESENTATION(#6902,#6791);
#6718=PROPERTY_DEFINITION_REPRESENTATION(#6903,#6792);
#6719=PROPERTY_DEFINITION_REPRESENTATION(#6904,#6793);
#6720=PROPERTY_DEFINITION_REPRESENTATION(#6905,#6794);
#6721=PROPERTY_DEFINITION_REPRESENTATION(#6906,#6795);
#6722=PROPERTY_DEFINITION_REPRESENTATION(#6907,#6796);
#6723=PROPERTY_DEFINITION_REPRESENTATION(#6908,#6797);
#6724=PROPERTY_DEFINITION_REPRESENTATION(#6909,#6798);
#6725=PROPERTY_DEFINITION_REPRESENTATION(#6910,#6799);
#6726=PROPERTY_DEFINITION_REPRESENTATION(#6911,#6800);
#6727=PROPERTY_DEFINITION_REPRESENTATION(#6912,#6801);
#6728=PROPERTY_DEFINITION_REPRESENTATION(#6913,#6802);
#6729=PROPERTY_DEFINITION_REPRESENTATION(#6914,#6803);
#6730=PROPERTY_DEFINITION_REPRESENTATION(#6915,#6804);
#6731=PROPERTY_DEFINITION_REPRESENTATION(#6916,#6805);
#6732=PROPERTY_DEFINITION_REPRESENTATION(#6917,#6806);
#6733=PROPERTY_DEFINITION_REPRESENTATION(#6918,#6807);
#6734=PROPERTY_DEFINITION_REPRESENTATION(#6919,#6808);
#6735=PROPERTY_DEFINITION_REPRESENTATION(#6920,#6809);
#6736=PROPERTY_DEFINITION_REPRESENTATION(#6921,#6810);
#6737=PROPERTY_DEFINITION_REPRESENTATION(#6922,#6811);
#6738=PROPERTY_DEFINITION_REPRESENTATION(#6923,#6812);
#6739=PROPERTY_DEFINITION_REPRESENTATION(#6924,#6813);
#6740=PROPERTY_DEFINITION_REPRESENTATION(#6925,#6814);
#6741=PROPERTY_DEFINITION_REPRESENTATION(#6926,#6815);
#6742=PROPERTY_DEFINITION_REPRESENTATION(#6927,#6816);
#6743=PROPERTY_DEFINITION_REPRESENTATION(#6928,#6817);
#6744=PROPERTY_DEFINITION_REPRESENTATION(#6929,#6818);
#6745=PROPERTY_DEFINITION_REPRESENTATION(#6930,#6819);
#6746=PROPERTY_DEFINITION_REPRESENTATION(#6931,#6820);
#6747=PROPERTY_DEFINITION_REPRESENTATION(#6932,#6821);
#6748=PROPERTY_DEFINITION_REPRESENTATION(#6933,#6822);
#6749=PROPERTY_DEFINITION_REPRESENTATION(#6934,#6823);
#6750=PROPERTY_DEFINITION_REPRESENTATION(#6935,#6824);
#6751=PROPERTY_DEFINITION_REPRESENTATION(#6936,#6825);
#6752=PROPERTY_DEFINITION_REPRESENTATION(#6937,#6826);
#6753=PROPERTY_DEFINITION_REPRESENTATION(#6938,#6827);
#6754=PROPERTY_DEFINITION_REPRESENTATION(#6939,#6828);
#6755=PROPERTY_DEFINITION_REPRESENTATION(#6940,#6829);
#6756=PROPERTY_DEFINITION_REPRESENTATION(#6941,#6830);
#6757=PROPERTY_DEFINITION_REPRESENTATION(#6942,#6831);
#6758=PROPERTY_DEFINITION_REPRESENTATION(#6943,#6832);
#6759=PROPERTY_DEFINITION_REPRESENTATION(#6944,#6833);
#6760=PROPERTY_DEFINITION_REPRESENTATION(#6945,#6834);
#6761=PROPERTY_DEFINITION_REPRESENTATION(#6946,#6835);
#6762=PROPERTY_DEFINITION_REPRESENTATION(#6947,#6836);
#6763=PROPERTY_DEFINITION_REPRESENTATION(#6948,#6837);
#6764=PROPERTY_DEFINITION_REPRESENTATION(#6949,#6838);
#6765=PROPERTY_DEFINITION_REPRESENTATION(#6950,#6839);
#6766=PROPERTY_DEFINITION_REPRESENTATION(#6951,#6840);
#6767=PROPERTY_DEFINITION_REPRESENTATION(#6952,#6841);
#6768=PROPERTY_DEFINITION_REPRESENTATION(#6953,#6842);
#6769=PROPERTY_DEFINITION_REPRESENTATION(#6954,#6843);
#6770=PROPERTY_DEFINITION_REPRESENTATION(#6955,#6844);
#6771=PROPERTY_DEFINITION_REPRESENTATION(#6956,#6845);
#6772=PROPERTY_DEFINITION_REPRESENTATION(#6957,#6846);
#6773=PROPERTY_DEFINITION_REPRESENTATION(#6958,#6847);
#6774=PROPERTY_DEFINITION_REPRESENTATION(#6959,#6848);
#6775=REPRESENTATION('material name',(#6849),#12742);
#6776=REPRESENTATION('density',(#6664),#12742);
#6777=REPRESENTATION('material name',(#6850),#12743);
#6778=REPRESENTATION('density',(#6665),#12743);
#6779=REPRESENTATION('material name',(#6851),#12744);
#6780=REPRESENTATION('density',(#6666),#12744);
#6781=REPRESENTATION('material name',(#6852),#12745);
#6782=REPRESENTATION('density',(#6667),#12745);
#6783=REPRESENTATION('material name',(#6853),#12746);
#6784=REPRESENTATION('density',(#6668),#12746);
#6785=REPRESENTATION('material name',(#6854),#12747);
#6786=REPRESENTATION('density',(#6669),#12747);
#6787=REPRESENTATION('material name',(#6855),#12748);
#6788=REPRESENTATION('density',(#6670),#12748);
#6789=REPRESENTATION('material name',(#6856),#12750);
#6790=REPRESENTATION('density',(#6671),#12750);
#6791=REPRESENTATION('material name',(#6857),#12751);
#6792=REPRESENTATION('density',(#6672),#12751);
#6793=REPRESENTATION('material name',(#6858),#12752);
#6794=REPRESENTATION('density',(#6673),#12752);
#6795=REPRESENTATION('material name',(#6859),#12753);
#6796=REPRESENTATION('density',(#6674),#12753);
#6797=REPRESENTATION('material name',(#6860),#12754);
#6798=REPRESENTATION('density',(#6675),#12754);
#6799=REPRESENTATION('material name',(#6861),#12755);
#6800=REPRESENTATION('density',(#6676),#12755);
#6801=REPRESENTATION('material name',(#6862),#12756);
#6802=REPRESENTATION('density',(#6677),#12756);
#6803=REPRESENTATION('material name',(#6863),#12758);
#6804=REPRESENTATION('density',(#6678),#12758);
#6805=REPRESENTATION('material name',(#6864),#12759);
#6806=REPRESENTATION('density',(#6679),#12759);
#6807=REPRESENTATION('material name',(#6865),#12760);
#6808=REPRESENTATION('density',(#6680),#12760);
#6809=REPRESENTATION('material name',(#6866),#12761);
#6810=REPRESENTATION('density',(#6681),#12761);
#6811=REPRESENTATION('material name',(#6867),#12762);
#6812=REPRESENTATION('density',(#6682),#12762);
#6813=REPRESENTATION('material name',(#6868),#12763);
#6814=REPRESENTATION('density',(#6683),#12763);
#6815=REPRESENTATION('material name',(#6869),#12764);
#6816=REPRESENTATION('density',(#6684),#12764);
#6817=REPRESENTATION('material name',(#6870),#12765);
#6818=REPRESENTATION('density',(#6685),#12765);
#6819=REPRESENTATION('material name',(#6871),#12766);
#6820=REPRESENTATION('density',(#6686),#12766);
#6821=REPRESENTATION('material name',(#6872),#12768);
#6822=REPRESENTATION('density',(#6687),#12768);
#6823=REPRESENTATION('material name',(#6873),#12769);
#6824=REPRESENTATION('density',(#6688),#12769);
#6825=REPRESENTATION('material name',(#6874),#12770);
#6826=REPRESENTATION('density',(#6689),#12770);
#6827=REPRESENTATION('material name',(#6875),#12771);
#6828=REPRESENTATION('density',(#6690),#12771);
#6829=REPRESENTATION('material name',(#6876),#12772);
#6830=REPRESENTATION('density',(#6691),#12772);
#6831=REPRESENTATION('material name',(#6877),#12774);
#6832=REPRESENTATION('density',(#6692),#12774);
#6833=REPRESENTATION('material name',(#6878),#12775);
#6834=REPRESENTATION('density',(#6693),#12775);
#6835=REPRESENTATION('material name',(#6879),#12776);
#6836=REPRESENTATION('density',(#6694),#12776);
#6837=REPRESENTATION('material name',(#6880),#12777);
#6838=REPRESENTATION('density',(#6695),#12777);
#6839=REPRESENTATION('material name',(#6881),#12778);
#6840=REPRESENTATION('density',(#6696),#12778);
#6841=REPRESENTATION('material name',(#6882),#12779);
#6842=REPRESENTATION('density',(#6697),#12779);
#6843=REPRESENTATION('material name',(#6883),#12780);
#6844=REPRESENTATION('density',(#6698),#12780);
#6845=REPRESENTATION('material name',(#6884),#12781);
#6846=REPRESENTATION('density',(#6699),#12781);
#6847=REPRESENTATION('material name',(#6885),#12782);
#6848=REPRESENTATION('density',(#6700),#12782);
#6849=DESCRIPTIVE_REPRESENTATION_ITEM('Steel','Steel');
#6850=DESCRIPTIVE_REPRESENTATION_ITEM('Steel','Steel');
#6851=DESCRIPTIVE_REPRESENTATION_ITEM('Steel','Steel');
#6852=DESCRIPTIVE_REPRESENTATION_ITEM('Steel','Steel');
#6853=DESCRIPTIVE_REPRESENTATION_ITEM('Steel','Steel');
#6854=DESCRIPTIVE_REPRESENTATION_ITEM('Steel','Steel');
#6855=DESCRIPTIVE_REPRESENTATION_ITEM('Steel','Steel');
#6856=DESCRIPTIVE_REPRESENTATION_ITEM('Steel','Steel');
#6857=DESCRIPTIVE_REPRESENTATION_ITEM('Steel','Steel');
#6858=DESCRIPTIVE_REPRESENTATION_ITEM('Steel','Steel');
#6859=DESCRIPTIVE_REPRESENTATION_ITEM('Steel','Steel');
#6860=DESCRIPTIVE_REPRESENTATION_ITEM('Steel','Steel');
#6861=DESCRIPTIVE_REPRESENTATION_ITEM('Steel','Steel');
#6862=DESCRIPTIVE_REPRESENTATION_ITEM('Steel','Steel');
#6863=DESCRIPTIVE_REPRESENTATION_ITEM('Steel','Steel');
#6864=DESCRIPTIVE_REPRESENTATION_ITEM('Steel','Steel');
#6865=DESCRIPTIVE_REPRESENTATION_ITEM('Steel','Steel');
#6866=DESCRIPTIVE_REPRESENTATION_ITEM('Steel','Steel');
#6867=DESCRIPTIVE_REPRESENTATION_ITEM('Steel','Steel');
#6868=DESCRIPTIVE_REPRESENTATION_ITEM('Steel','Steel');
#6869=DESCRIPTIVE_REPRESENTATION_ITEM('Steel','Steel');
#6870=DESCRIPTIVE_REPRESENTATION_ITEM('Steel','Steel');
#6871=DESCRIPTIVE_REPRESENTATION_ITEM('Steel','Steel');
#6872=DESCRIPTIVE_REPRESENTATION_ITEM('Steel','Steel');
#6873=DESCRIPTIVE_REPRESENTATION_ITEM('Steel','Steel');
#6874=DESCRIPTIVE_REPRESENTATION_ITEM('Steel','Steel');
#6875=DESCRIPTIVE_REPRESENTATION_ITEM('Steel','Steel');
#6876=DESCRIPTIVE_REPRESENTATION_ITEM('Steel','Steel');
#6877=DESCRIPTIVE_REPRESENTATION_ITEM('Steel','Steel');
#6878=DESCRIPTIVE_REPRESENTATION_ITEM('Steel','Steel');
#6879=DESCRIPTIVE_REPRESENTATION_ITEM('Steel','Steel');
#6880=DESCRIPTIVE_REPRESENTATION_ITEM('Steel','Steel');
#6881=DESCRIPTIVE_REPRESENTATION_ITEM('Steel','Steel');
#6882=DESCRIPTIVE_REPRESENTATION_ITEM('Steel','Steel');
#6883=DESCRIPTIVE_REPRESENTATION_ITEM('Steel','Steel');
#6884=DESCRIPTIVE_REPRESENTATION_ITEM('Steel','Steel');
#6885=DESCRIPTIVE_REPRESENTATION_ITEM('Steel','Steel');
#6886=PROPERTY_DEFINITION('material property','material name',#12977);
#6887=PROPERTY_DEFINITION('material property','density of part',#12977);
#6888=PROPERTY_DEFINITION('material property','material name',#12978);
#6889=PROPERTY_DEFINITION('material property','density of part',#12978);
#6890=PROPERTY_DEFINITION('material property','material name',#12979);
#6891=PROPERTY_DEFINITION('material property','density of part',#12979);
#6892=PROPERTY_DEFINITION('material property','material name',#12980);
#6893=PROPERTY_DEFINITION('material property','density of part',#12980);
#6894=PROPERTY_DEFINITION('material property','material name',#12981);
#6895=PROPERTY_DEFINITION('material property','density of part',#12981);
#6896=PROPERTY_DEFINITION('material property','material name',#12982);
#6897=PROPERTY_DEFINITION('material property','density of part',#12982);
#6898=PROPERTY_DEFINITION('material property','material name',#12983);
#6899=PROPERTY_DEFINITION('material property','density of part',#12983);
#6900=PROPERTY_DEFINITION('material property','material name',#12985);
#6901=PROPERTY_DEFINITION('material property','density of part',#12985);
#6902=PROPERTY_DEFINITION('material property','material name',#12986);
#6903=PROPERTY_DEFINITION('material property','density of part',#12986);
#6904=PROPERTY_DEFINITION('material property','material name',#12987);
#6905=PROPERTY_DEFINITION('material property','density of part',#12987);
#6906=PROPERTY_DEFINITION('material property','material name',#12988);
#6907=PROPERTY_DEFINITION('material property','density of part',#12988);
#6908=PROPERTY_DEFINITION('material property','material name',#12989);
#6909=PROPERTY_DEFINITION('material property','density of part',#12989);
#6910=PROPERTY_DEFINITION('material property','material name',#12990);
#6911=PROPERTY_DEFINITION('material property','density of part',#12990);
#6912=PROPERTY_DEFINITION('material property','material name',#12991);
#6913=PROPERTY_DEFINITION('material property','density of part',#12991);
#6914=PROPERTY_DEFINITION('material property','material name',#12993);
#6915=PROPERTY_DEFINITION('material property','density of part',#12993);
#6916=PROPERTY_DEFINITION('material property','material name',#12994);
#6917=PROPERTY_DEFINITION('material property','density of part',#12994);
#6918=PROPERTY_DEFINITION('material property','material name',#12995);
#6919=PROPERTY_DEFINITION('material property','density of part',#12995);
#6920=PROPERTY_DEFINITION('material property','material name',#12996);
#6921=PROPERTY_DEFINITION('material property','density of part',#12996);
#6922=PROPERTY_DEFINITION('material property','material name',#12997);
#6923=PROPERTY_DEFINITION('material property','density of part',#12997);
#6924=PROPERTY_DEFINITION('material property','material name',#12998);
#6925=PROPERTY_DEFINITION('material property','density of part',#12998);
#6926=PROPERTY_DEFINITION('material property','material name',#12999);
#6927=PROPERTY_DEFINITION('material property','density of part',#12999);
#6928=PROPERTY_DEFINITION('material property','material name',#13000);
#6929=PROPERTY_DEFINITION('material property','density of part',#13000);
#6930=PROPERTY_DEFINITION('material property','material name',#13001);
#6931=PROPERTY_DEFINITION('material property','density of part',#13001);
#6932=PROPERTY_DEFINITION('material property','material name',#13003);
#6933=PROPERTY_DEFINITION('material property','density of part',#13003);
#6934=PROPERTY_DEFINITION('material property','material name',#13004);
#6935=PROPERTY_DEFINITION('material property','density of part',#13004);
#6936=PROPERTY_DEFINITION('material property','material name',#13005);
#6937=PROPERTY_DEFINITION('material property','density of part',#13005);
#6938=PROPERTY_DEFINITION('material property','material name',#13006);
#6939=PROPERTY_DEFINITION('material property','density of part',#13006);
#6940=PROPERTY_DEFINITION('material property','material name',#13007);
#6941=PROPERTY_DEFINITION('material property','density of part',#13007);
#6942=PROPERTY_DEFINITION('material property','material name',#13009);
#6943=PROPERTY_DEFINITION('material property','density of part',#13009);
#6944=PROPERTY_DEFINITION('material property','material name',#13010);
#6945=PROPERTY_DEFINITION('material property','density of part',#13010);
#6946=PROPERTY_DEFINITION('material property','material name',#13011);
#6947=PROPERTY_DEFINITION('material property','density of part',#13011);
#6948=PROPERTY_DEFINITION('material property','material name',#13012);
#6949=PROPERTY_DEFINITION('material property','density of part',#13012);
#6950=PROPERTY_DEFINITION('material property','material name',#13013);
#6951=PROPERTY_DEFINITION('material property','density of part',#13013);
#6952=PROPERTY_DEFINITION('material property','material name',#13014);
#6953=PROPERTY_DEFINITION('material property','density of part',#13014);
#6954=PROPERTY_DEFINITION('material property','material name',#13015);
#6955=PROPERTY_DEFINITION('material property','density of part',#13015);
#6956=PROPERTY_DEFINITION('material property','material name',#13016);
#6957=PROPERTY_DEFINITION('material property','density of part',#13016);
#6958=PROPERTY_DEFINITION('material property','material name',#13017);
#6959=PROPERTY_DEFINITION('material property','density of part',#13017);
#6960=AXIS2_PLACEMENT_3D('',#9925,#7810,#7811);
#6961=AXIS2_PLACEMENT_3D('',#9926,#7812,#7813);
#6962=AXIS2_PLACEMENT_3D('',#9927,#7814,#7815);
#6963=AXIS2_PLACEMENT_3D('',#9928,#7816,#7817);
#6964=AXIS2_PLACEMENT_3D('',#9930,#7818,#7819);
#6965=AXIS2_PLACEMENT_3D('',#9933,#7821,#7822);
#6966=AXIS2_PLACEMENT_3D('',#9934,#7823,#7824);
#6967=AXIS2_PLACEMENT_3D('',#9936,#7825,#7826);
#6968=AXIS2_PLACEMENT_3D('',#9939,#7828,#7829);
#6969=AXIS2_PLACEMENT_3D('',#9940,#7830,#7831);
#6970=AXIS2_PLACEMENT_3D('',#9942,#7832,#7833);
#6971=AXIS2_PLACEMENT_3D('',#9945,#7835,#7836);
#6972=AXIS2_PLACEMENT_3D('',#9946,#7837,#7838);
#6973=AXIS2_PLACEMENT_3D('',#9948,#7839,#7840);
#6974=AXIS2_PLACEMENT_3D('',#9951,#7842,#7843);
#6975=AXIS2_PLACEMENT_3D('',#9952,#7844,#7845);
#6976=AXIS2_PLACEMENT_3D('',#9961,#7850,#7851);
#6977=AXIS2_PLACEMENT_3D('',#9967,#7855,#7856);
#6978=AXIS2_PLACEMENT_3D('',#9973,#7860,#7861);
#6979=AXIS2_PLACEMENT_3D('',#9976,#7864,#7865);
#6980=AXIS2_PLACEMENT_3D('',#9977,#7866,#7867);
#6981=AXIS2_PLACEMENT_3D('',#9978,#7868,#7869);
#6982=AXIS2_PLACEMENT_3D('',#9979,#7870,#7871);
#6983=AXIS2_PLACEMENT_3D('',#9981,#7872,#7873);
#6984=AXIS2_PLACEMENT_3D('',#9984,#7875,#7876);
#6985=AXIS2_PLACEMENT_3D('',#9985,#7877,#7878);
#6986=AXIS2_PLACEMENT_3D('',#9986,#7879,#7880);
#6987=AXIS2_PLACEMENT_3D('',#9988,#7881,#7882);
#6988=AXIS2_PLACEMENT_3D('',#9991,#7884,#7885);
#6989=AXIS2_PLACEMENT_3D('',#9992,#7886,#7887);
#6990=AXIS2_PLACEMENT_3D('',#9993,#7888,#7889);
#6991=AXIS2_PLACEMENT_3D('',#9995,#7890,#7891);
#6992=AXIS2_PLACEMENT_3D('',#9998,#7893,#7894);
#6993=AXIS2_PLACEMENT_3D('',#9999,#7895,#7896);
#6994=AXIS2_PLACEMENT_3D('',#10000,#7897,#7898);
#6995=AXIS2_PLACEMENT_3D('',#10002,#7899,#7900);
#6996=AXIS2_PLACEMENT_3D('',#10005,#7902,#7903);
#6997=AXIS2_PLACEMENT_3D('',#10006,#7904,#7905);
#6998=AXIS2_PLACEMENT_3D('',#10007,#7906,#7907);
#6999=AXIS2_PLACEMENT_3D('',#10009,#7908,#7909);
#7000=AXIS2_PLACEMENT_3D('',#10012,#7911,#7912);
#7001=AXIS2_PLACEMENT_3D('',#10013,#7913,#7914);
#7002=AXIS2_PLACEMENT_3D('',#10014,#7915,#7916);
#7003=AXIS2_PLACEMENT_3D('',#10016,#7917,#7918);
#7004=AXIS2_PLACEMENT_3D('',#10019,#7920,#7921);
#7005=AXIS2_PLACEMENT_3D('',#10020,#7922,#7923);
#7006=AXIS2_PLACEMENT_3D('',#10021,#7924,#7925);
#7007=AXIS2_PLACEMENT_3D('',#10023,#7926,#7927);
#7008=AXIS2_PLACEMENT_3D('',#10026,#7929,#7930);
#7009=AXIS2_PLACEMENT_3D('',#10027,#7931,#7932);
#7010=AXIS2_PLACEMENT_3D('',#10028,#7933,#7934);
#7011=AXIS2_PLACEMENT_3D('',#10030,#7935,#7936);
#7012=AXIS2_PLACEMENT_3D('',#10033,#7938,#7939);
#7013=AXIS2_PLACEMENT_3D('',#10034,#7940,#7941);
#7014=AXIS2_PLACEMENT_3D('',#10035,#7942,#7943);
#7015=AXIS2_PLACEMENT_3D('',#10040,#7945,#7946);
#7016=AXIS2_PLACEMENT_3D('',#10043,#7948,#7949);
#7017=AXIS2_PLACEMENT_3D('',#10044,#7950,#7951);
#7018=AXIS2_PLACEMENT_3D('',#10049,#7953,#7954);
#7019=AXIS2_PLACEMENT_3D('',#10052,#7956,#7957);
#7020=AXIS2_PLACEMENT_3D('',#10053,#7958,#7959);
#7021=AXIS2_PLACEMENT_3D('',#10057,#7962,#7963);
#7022=AXIS2_PLACEMENT_3D('',#10058,#7964,#7965);
#7023=AXIS2_PLACEMENT_3D('',#10063,#7967,#7968);
#7024=AXIS2_PLACEMENT_3D('',#10066,#7970,#7971);
#7025=AXIS2_PLACEMENT_3D('',#10067,#7972,#7973);
#7026=AXIS2_PLACEMENT_3D('',#10072,#7975,#7976);
#7027=AXIS2_PLACEMENT_3D('',#10075,#7978,#7979);
#7028=AXIS2_PLACEMENT_3D('',#10076,#7980,#7981);
#7029=AXIS2_PLACEMENT_3D('',#10080,#7984,#7985);
#7030=AXIS2_PLACEMENT_3D('',#10081,#7986,#7987);
#7031=AXIS2_PLACEMENT_3D('',#10086,#7989,#7990);
#7032=AXIS2_PLACEMENT_3D('',#10089,#7992,#7993);
#7033=AXIS2_PLACEMENT_3D('',#10090,#7994,#7995);
#7034=AXIS2_PLACEMENT_3D('',#10095,#7997,#7998);
#7035=AXIS2_PLACEMENT_3D('',#10098,#8000,#8001);
#7036=AXIS2_PLACEMENT_3D('',#10099,#8002,#8003);
#7037=AXIS2_PLACEMENT_3D('',#10103,#8006,#8007);
#7038=AXIS2_PLACEMENT_3D('',#10104,#8008,#8009);
#7039=AXIS2_PLACEMENT_3D('',#10109,#8011,#8012);
#7040=AXIS2_PLACEMENT_3D('',#10112,#8014,#8015);
#7041=AXIS2_PLACEMENT_3D('',#10113,#8016,#8017);
#7042=AXIS2_PLACEMENT_3D('',#10118,#8019,#8020);
#7043=AXIS2_PLACEMENT_3D('',#10121,#8022,#8023);
#7044=AXIS2_PLACEMENT_3D('',#10122,#8024,#8025);
#7045=AXIS2_PLACEMENT_3D('',#10126,#8028,#8029);
#7046=AXIS2_PLACEMENT_3D('',#10127,#8030,#8031);
#7047=AXIS2_PLACEMENT_3D('',#10133,#8035,#8036);
#7048=AXIS2_PLACEMENT_3D('',#10139,#8040,#8041);
#7049=AXIS2_PLACEMENT_3D('',#10145,#8045,#8046);
#7050=AXIS2_PLACEMENT_3D('',#10151,#8050,#8051);
#7051=AXIS2_PLACEMENT_3D('',#10161,#8057,#8058);
#7052=AXIS2_PLACEMENT_3D('',#10162,#8059,#8060);
#7053=AXIS2_PLACEMENT_3D('',#10166,#8063,#8064);
#7054=AXIS2_PLACEMENT_3D('',#10170,#8067,#8068);
#7055=AXIS2_PLACEMENT_3D('',#10172,#8069,#8070);
#7056=AXIS2_PLACEMENT_3D('',#10181,#8076,#8077);
#7057=AXIS2_PLACEMENT_3D('',#10185,#8080,#8081);
#7058=AXIS2_PLACEMENT_3D('',#10189,#8084,#8085);
#7059=AXIS2_PLACEMENT_3D('',#10191,#8086,#8087);
#7060=AXIS2_PLACEMENT_3D('',#10193,#8089,#8090);
#7061=AXIS2_PLACEMENT_3D('',#10195,#8091,#8092);
#7062=AXIS2_PLACEMENT_3D('',#10197,#8094,#8095);
#7063=AXIS2_PLACEMENT_3D('',#10199,#8096,#8097);
#7064=AXIS2_PLACEMENT_3D('',#10201,#8099,#8100);
#7065=AXIS2_PLACEMENT_3D('',#10203,#8101,#8102);
#7066=AXIS2_PLACEMENT_3D('',#10205,#8104,#8105);
#7067=AXIS2_PLACEMENT_3D('',#10209,#8108,#8109);
#7068=AXIS2_PLACEMENT_3D('',#10213,#8112,#8113);
#7069=AXIS2_PLACEMENT_3D('',#10215,#8115,#8116);
#7070=AXIS2_PLACEMENT_3D('',#10216,#8117,#8118);
#7071=AXIS2_PLACEMENT_3D('',#10217,#8119,#8120);
#7072=AXIS2_PLACEMENT_3D('',#10221,#8123,#8124);
#7073=AXIS2_PLACEMENT_3D('',#10225,#8127,#8128);
#7074=AXIS2_PLACEMENT_3D('',#10227,#8130,#8131);
#7075=AXIS2_PLACEMENT_3D('',#10228,#8132,#8133);
#7076=AXIS2_PLACEMENT_3D('',#10229,#8134,#8135);
#7077=AXIS2_PLACEMENT_3D('',#10231,#8136,#8137);
#7078=AXIS2_PLACEMENT_3D('',#10234,#8139,#8140);
#7079=AXIS2_PLACEMENT_3D('',#10235,#8141,#8142);
#7080=AXIS2_PLACEMENT_3D('',#10237,#8143,#8144);
#7081=AXIS2_PLACEMENT_3D('',#10240,#8146,#8147);
#7082=AXIS2_PLACEMENT_3D('',#10241,#8148,#8149);
#7083=AXIS2_PLACEMENT_3D('',#10242,#8150,#8151);
#7084=AXIS2_PLACEMENT_3D('',#10243,#8152,#8153);
#7085=AXIS2_PLACEMENT_3D('',#10244,#8154,#8155);
#7086=AXIS2_PLACEMENT_3D('',#10246,#8156,#8157);
#7087=AXIS2_PLACEMENT_3D('',#10249,#8159,#8160);
#7088=AXIS2_PLACEMENT_3D('',#10250,#8161,#8162);
#7089=AXIS2_PLACEMENT_3D('',#10252,#8163,#8164);
#7090=AXIS2_PLACEMENT_3D('',#10255,#8166,#8167);
#7091=AXIS2_PLACEMENT_3D('',#10256,#8168,#8169);
#7092=AXIS2_PLACEMENT_3D('',#10257,#8170,#8171);
#7093=AXIS2_PLACEMENT_3D('',#10258,#8172,#8173);
#7094=AXIS2_PLACEMENT_3D('',#10259,#8174,#8175);
#7095=AXIS2_PLACEMENT_3D('',#10261,#8176,#8177);
#7096=AXIS2_PLACEMENT_3D('',#10264,#8179,#8180);
#7097=AXIS2_PLACEMENT_3D('',#10265,#8181,#8182);
#7098=AXIS2_PLACEMENT_3D('',#10267,#8183,#8184);
#7099=AXIS2_PLACEMENT_3D('',#10270,#8186,#8187);
#7100=AXIS2_PLACEMENT_3D('',#10271,#8188,#8189);
#7101=AXIS2_PLACEMENT_3D('',#10273,#8190,#8191);
#7102=AXIS2_PLACEMENT_3D('',#10276,#8193,#8194);
#7103=AXIS2_PLACEMENT_3D('',#10277,#8195,#8196);
#7104=AXIS2_PLACEMENT_3D('',#10279,#8197,#8198);
#7105=AXIS2_PLACEMENT_3D('',#10282,#8200,#8201);
#7106=AXIS2_PLACEMENT_3D('',#10283,#8202,#8203);
#7107=AXIS2_PLACEMENT_3D('',#10285,#8204,#8205);
#7108=AXIS2_PLACEMENT_3D('',#10288,#8207,#8208);
#7109=AXIS2_PLACEMENT_3D('',#10289,#8209,#8210);
#7110=AXIS2_PLACEMENT_3D('',#10291,#8211,#8212);
#7111=AXIS2_PLACEMENT_3D('',#10292,#8213,#8214);
#7112=AXIS2_PLACEMENT_3D('',#10295,#8216,#8217);
#7113=AXIS2_PLACEMENT_3D('',#10296,#8218,#8219);
#7114=AXIS2_PLACEMENT_3D('',#10298,#8220,#8221);
#7115=AXIS2_PLACEMENT_3D('',#10301,#8223,#8224);
#7116=AXIS2_PLACEMENT_3D('',#10302,#8225,#8226);
#7117=AXIS2_PLACEMENT_3D('',#10303,#8227,#8228);
#7118=AXIS2_PLACEMENT_3D('',#10304,#8229,#8230);
#7119=AXIS2_PLACEMENT_3D('',#10305,#8231,#8232);
#7120=AXIS2_PLACEMENT_3D('',#10307,#8233,#8234);
#7121=AXIS2_PLACEMENT_3D('',#10310,#8236,#8237);
#7122=AXIS2_PLACEMENT_3D('',#10311,#8238,#8239);
#7123=AXIS2_PLACEMENT_3D('',#10313,#8240,#8241);
#7124=AXIS2_PLACEMENT_3D('',#10316,#8243,#8244);
#7125=AXIS2_PLACEMENT_3D('',#10317,#8245,#8246);
#7126=AXIS2_PLACEMENT_3D('',#10319,#8247,#8248);
#7127=AXIS2_PLACEMENT_3D('',#10322,#8250,#8251);
#7128=AXIS2_PLACEMENT_3D('',#10323,#8252,#8253);
#7129=AXIS2_PLACEMENT_3D('',#10325,#8254,#8255);
#7130=AXIS2_PLACEMENT_3D('',#10328,#8257,#8258);
#7131=AXIS2_PLACEMENT_3D('',#10329,#8259,#8260);
#7132=AXIS2_PLACEMENT_3D('',#10331,#8261,#8262);
#7133=AXIS2_PLACEMENT_3D('',#10334,#8264,#8265);
#7134=AXIS2_PLACEMENT_3D('',#10335,#8266,#8267);
#7135=AXIS2_PLACEMENT_3D('',#10337,#8268,#8269);
#7136=AXIS2_PLACEMENT_3D('',#10338,#8270,#8271);
#7137=AXIS2_PLACEMENT_3D('',#10340,#8272,#8273);
#7138=AXIS2_PLACEMENT_3D('',#10342,#8275,#8276);
#7139=AXIS2_PLACEMENT_3D('',#10344,#8277,#8278);
#7140=AXIS2_PLACEMENT_3D('',#10347,#8280,#8281);
#7141=AXIS2_PLACEMENT_3D('',#10348,#8282,#8283);
#7142=AXIS2_PLACEMENT_3D('',#10349,#8284,#8285);
#7143=AXIS2_PLACEMENT_3D('',#10350,#8286,#8287);
#7144=AXIS2_PLACEMENT_3D('',#10351,#8288,#8289);
#7145=AXIS2_PLACEMENT_3D('',#10360,#8294,#8295);
#7146=AXIS2_PLACEMENT_3D('',#10366,#8299,#8300);
#7147=AXIS2_PLACEMENT_3D('',#10372,#8304,#8305);
#7148=AXIS2_PLACEMENT_3D('',#10375,#8308,#8309);
#7149=AXIS2_PLACEMENT_3D('',#10376,#8310,#8311);
#7150=AXIS2_PLACEMENT_3D('',#10377,#8312,#8313);
#7151=AXIS2_PLACEMENT_3D('',#10378,#8314,#8315);
#7152=AXIS2_PLACEMENT_3D('',#10387,#8320,#8321);
#7153=AXIS2_PLACEMENT_3D('',#10393,#8325,#8326);
#7154=AXIS2_PLACEMENT_3D('',#10399,#8330,#8331);
#7155=AXIS2_PLACEMENT_3D('',#10402,#8334,#8335);
#7156=AXIS2_PLACEMENT_3D('',#10403,#8336,#8337);
#7157=AXIS2_PLACEMENT_3D('',#10404,#8338,#8339);
#7158=AXIS2_PLACEMENT_3D('',#10405,#8340,#8341);
#7159=AXIS2_PLACEMENT_3D('',#10406,#8342,#8343);
#7160=AXIS2_PLACEMENT_3D('',#10409,#8344,#8345);
#7161=AXIS2_PLACEMENT_3D('',#10410,#8346,#8347);
#7162=AXIS2_PLACEMENT_3D('',#10412,#8348,#8349);
#7163=AXIS2_PLACEMENT_3D('',#10414,#8350,#8351);
#7164=AXIS2_PLACEMENT_3D('',#10415,#8352,#8353);
#7165=AXIS2_PLACEMENT_3D('',#10416,#8354,#8355);
#7166=AXIS2_PLACEMENT_3D('',#10419,#8357,#8358);
#7167=AXIS2_PLACEMENT_3D('',#10420,#8359,#8360);
#7168=AXIS2_PLACEMENT_3D('',#10422,#8361,#8362);
#7169=AXIS2_PLACEMENT_3D('',#10425,#8364,#8365);
#7170=AXIS2_PLACEMENT_3D('',#10426,#8366,#8367);
#7171=AXIS2_PLACEMENT_3D('',#10429,#8369,#8370);
#7172=AXIS2_PLACEMENT_3D('',#10430,#8371,#8372);
#7173=AXIS2_PLACEMENT_3D('',#10431,#8373,#8374);
#7174=AXIS2_PLACEMENT_3D('',#10433,#8375,#8376);
#7175=AXIS2_PLACEMENT_3D('',#10435,#8378,#8379);
#7176=AXIS2_PLACEMENT_3D('',#10437,#8380,#8381);
#7177=AXIS2_PLACEMENT_3D('',#10438,#8382,#8383);
#7178=AXIS2_PLACEMENT_3D('',#10440,#8385,#8386);
#7179=AXIS2_PLACEMENT_3D('',#10441,#8387,#8388);
#7180=AXIS2_PLACEMENT_3D('',#10444,#8389,#8390);
#7181=AXIS2_PLACEMENT_3D('',#10445,#8391,#8392);
#7182=AXIS2_PLACEMENT_3D('',#10447,#8393,#8394);
#7183=AXIS2_PLACEMENT_3D('',#10449,#8395,#8396);
#7184=AXIS2_PLACEMENT_3D('',#10450,#8397,#8398);
#7185=AXIS2_PLACEMENT_3D('',#10451,#8399,#8400);
#7186=AXIS2_PLACEMENT_3D('',#10453,#8401,#8402);
#7187=AXIS2_PLACEMENT_3D('',#10455,#8404,#8405);
#7188=AXIS2_PLACEMENT_3D('',#10457,#8406,#8407);
#7189=AXIS2_PLACEMENT_3D('',#10459,#8408,#8409);
#7190=AXIS2_PLACEMENT_3D('',#10460,#8410,#8411);
#7191=AXIS2_PLACEMENT_3D('',#10462,#8412,#8413);
#7192=AXIS2_PLACEMENT_3D('',#10464,#8415,#8416);
#7193=AXIS2_PLACEMENT_3D('',#10466,#8417,#8418);
#7194=AXIS2_PLACEMENT_3D('',#10468,#8420,#8421);
#7195=AXIS2_PLACEMENT_3D('',#10470,#8422,#8423);
#7196=AXIS2_PLACEMENT_3D('',#10472,#8425,#8426);
#7197=AXIS2_PLACEMENT_3D('',#10473,#8427,#8428);
#7198=AXIS2_PLACEMENT_3D('',#10475,#8430,#8431);
#7199=AXIS2_PLACEMENT_3D('',#10476,#8432,#8433);
#7200=AXIS2_PLACEMENT_3D('',#10479,#8434,#8435);
#7201=AXIS2_PLACEMENT_3D('',#10480,#8436,#8437);
#7202=AXIS2_PLACEMENT_3D('',#10483,#8438,#8439);
#7203=AXIS2_PLACEMENT_3D('',#10484,#8440,#8441);
#7204=AXIS2_PLACEMENT_3D('',#10487,#8442,#8443);
#7205=AXIS2_PLACEMENT_3D('',#10488,#8444,#8445);
#7206=AXIS2_PLACEMENT_3D('',#10491,#8446,#8447);
#7207=AXIS2_PLACEMENT_3D('',#10492,#8448,#8449);
#7208=AXIS2_PLACEMENT_3D('',#10495,#8450,#8451);
#7209=AXIS2_PLACEMENT_3D('',#10496,#8452,#8453);
#7210=AXIS2_PLACEMENT_3D('',#10499,#8454,#8455);
#7211=AXIS2_PLACEMENT_3D('',#10500,#8456,#8457);
#7212=AXIS2_PLACEMENT_3D('',#10503,#8458,#8459);
#7213=AXIS2_PLACEMENT_3D('',#10504,#8460,#8461);
#7214=AXIS2_PLACEMENT_3D('',#10507,#8462,#8463);
#7215=AXIS2_PLACEMENT_3D('',#10508,#8464,#8465);
#7216=AXIS2_PLACEMENT_3D('',#10511,#8466,#8467);
#7217=AXIS2_PLACEMENT_3D('',#10512,#8468,#8469);
#7218=AXIS2_PLACEMENT_3D('',#10513,#8470,#8471);
#7219=AXIS2_PLACEMENT_3D('',#10539,#8472,#8473);
#7220=AXIS2_PLACEMENT_3D('',#10563,#8474,#8475);
#7221=AXIS2_PLACEMENT_3D('',#10564,#8476,#8477);
#7222=AXIS2_PLACEMENT_3D('',#10566,#8478,#8479);
#7223=AXIS2_PLACEMENT_3D('',#10591,#8480,#8481);
#7224=AXIS2_PLACEMENT_3D('',#10616,#8482,#8483);
#7225=AXIS2_PLACEMENT_3D('',#10641,#8484,#8485);
#7226=AXIS2_PLACEMENT_3D('',#10644,#8487,#8488);
#7227=AXIS2_PLACEMENT_3D('',#10646,#8489,#8490);
#7228=AXIS2_PLACEMENT_3D('',#10671,#8491,#8492);
#7229=AXIS2_PLACEMENT_3D('',#10696,#8493,#8494);
#7230=AXIS2_PLACEMENT_3D('',#10721,#8495,#8496);
#7231=AXIS2_PLACEMENT_3D('',#10746,#8497,#8498);
#7232=AXIS2_PLACEMENT_3D('',#10770,#8499,#8500);
#7233=AXIS2_PLACEMENT_3D('',#10771,#8501,#8502);
#7234=AXIS2_PLACEMENT_3D('',#10773,#8503,#8504);
#7235=AXIS2_PLACEMENT_3D('',#10774,#8505,#8506);
#7236=AXIS2_PLACEMENT_3D('',#10775,#8507,#8508);
#7237=AXIS2_PLACEMENT_3D('',#10799,#8509,#8510);
#7238=AXIS2_PLACEMENT_3D('',#10800,#8511,#8512);
#7239=AXIS2_PLACEMENT_3D('',#10802,#8513,#8514);
#7240=AXIS2_PLACEMENT_3D('',#10803,#8515,#8516);
#7241=AXIS2_PLACEMENT_3D('',#10804,#8517,#8518);
#7242=AXIS2_PLACEMENT_3D('',#10828,#8519,#8520);
#7243=AXIS2_PLACEMENT_3D('',#10829,#8521,#8522);
#7244=AXIS2_PLACEMENT_3D('',#10831,#8523,#8524);
#7245=AXIS2_PLACEMENT_3D('',#10832,#8525,#8526);
#7246=AXIS2_PLACEMENT_3D('',#10833,#8527,#8528);
#7247=AXIS2_PLACEMENT_3D('',#10857,#8529,#8530);
#7248=AXIS2_PLACEMENT_3D('',#10858,#8531,#8532);
#7249=AXIS2_PLACEMENT_3D('',#10860,#8533,#8534);
#7250=AXIS2_PLACEMENT_3D('',#10862,#8535,#8536);
#7251=AXIS2_PLACEMENT_3D('',#10863,#8537,#8538);
#7252=AXIS2_PLACEMENT_3D('',#10864,#8539,#8540);
#7253=AXIS2_PLACEMENT_3D('',#10888,#8541,#8542);
#7254=AXIS2_PLACEMENT_3D('',#10889,#8543,#8544);
#7255=AXIS2_PLACEMENT_3D('',#10891,#8545,#8546);
#7256=AXIS2_PLACEMENT_3D('',#10892,#8547,#8548);
#7257=AXIS2_PLACEMENT_3D('',#10893,#8549,#8550);
#7258=AXIS2_PLACEMENT_3D('',#10917,#8551,#8552);
#7259=AXIS2_PLACEMENT_3D('',#10918,#8553,#8554);
#7260=AXIS2_PLACEMENT_3D('',#10920,#8555,#8556);
#7261=AXIS2_PLACEMENT_3D('',#10921,#8557,#8558);
#7262=AXIS2_PLACEMENT_3D('',#10922,#8559,#8560);
#7263=AXIS2_PLACEMENT_3D('',#10946,#8561,#8562);
#7264=AXIS2_PLACEMENT_3D('',#10947,#8563,#8564);
#7265=AXIS2_PLACEMENT_3D('',#10949,#8565,#8566);
#7266=AXIS2_PLACEMENT_3D('',#10950,#8567,#8568);
#7267=AXIS2_PLACEMENT_3D('',#10951,#8569,#8570);
#7268=AXIS2_PLACEMENT_3D('',#10975,#8571,#8572);
#7269=AXIS2_PLACEMENT_3D('',#10976,#8573,#8574);
#7270=AXIS2_PLACEMENT_3D('',#10978,#8575,#8576);
#7271=AXIS2_PLACEMENT_3D('',#10981,#8578,#8579);
#7272=AXIS2_PLACEMENT_3D('',#11005,#8580,#8581);
#7273=AXIS2_PLACEMENT_3D('',#11006,#8582,#8583);
#7274=AXIS2_PLACEMENT_3D('',#11007,#8584,#8585);
#7275=AXIS2_PLACEMENT_3D('',#11008,#8586,#8587);
#7276=AXIS2_PLACEMENT_3D('',#11009,#8588,#8589);
#7277=AXIS2_PLACEMENT_3D('',#11010,#8590,#8591);
#7278=AXIS2_PLACEMENT_3D('',#11011,#8592,#8593);
#7279=AXIS2_PLACEMENT_3D('',#11012,#8594,#8595);
#7280=AXIS2_PLACEMENT_3D('',#11013,#8596,#8597);
#7281=AXIS2_PLACEMENT_3D('',#11015,#8598,#8599);
#7282=AXIS2_PLACEMENT_3D('',#11017,#8600,#8601);
#7283=AXIS2_PLACEMENT_3D('',#11018,#8602,#8603);
#7284=AXIS2_PLACEMENT_3D('',#11020,#8604,#8605);
#7285=AXIS2_PLACEMENT_3D('',#11022,#8607,#8608);
#7286=AXIS2_PLACEMENT_3D('',#11024,#8609,#8610);
#7287=AXIS2_PLACEMENT_3D('',#11025,#8611,#8612);
#7288=AXIS2_PLACEMENT_3D('',#11027,#8614,#8615);
#7289=AXIS2_PLACEMENT_3D('',#11029,#8616,#8617);
#7290=AXIS2_PLACEMENT_3D('',#11031,#8618,#8619);
#7291=AXIS2_PLACEMENT_3D('',#11032,#8620,#8621);
#7292=AXIS2_PLACEMENT_3D('',#11034,#8622,#8623);
#7293=AXIS2_PLACEMENT_3D('',#11036,#8625,#8626);
#7294=AXIS2_PLACEMENT_3D('',#11038,#8627,#8628);
#7295=AXIS2_PLACEMENT_3D('',#11039,#8629,#8630);
#7296=AXIS2_PLACEMENT_3D('',#11041,#8632,#8633);
#7297=AXIS2_PLACEMENT_3D('',#11042,#8634,#8635);
#7298=AXIS2_PLACEMENT_3D('',#11043,#8636,#8637);
#7299=AXIS2_PLACEMENT_3D('',#11044,#8638,#8639);
#7300=AXIS2_PLACEMENT_3D('',#11045,#8640,#8641);
#7301=AXIS2_PLACEMENT_3D('',#11046,#8642,#8643);
#7302=AXIS2_PLACEMENT_3D('',#11047,#8644,#8645);
#7303=AXIS2_PLACEMENT_3D('',#11049,#8646,#8647);
#7304=AXIS2_PLACEMENT_3D('',#11050,#8648,#8649);
#7305=AXIS2_PLACEMENT_3D('',#11052,#8650,#8651);
#7306=AXIS2_PLACEMENT_3D('',#11054,#8653,#8654);
#7307=AXIS2_PLACEMENT_3D('',#11056,#8655,#8656);
#7308=AXIS2_PLACEMENT_3D('',#11058,#8658,#8659);
#7309=AXIS2_PLACEMENT_3D('',#11060,#8660,#8661);
#7310=AXIS2_PLACEMENT_3D('',#11062,#8663,#8664);
#7311=AXIS2_PLACEMENT_3D('',#11064,#8665,#8666);
#7312=AXIS2_PLACEMENT_3D('',#11065,#8667,#8668);
#7313=AXIS2_PLACEMENT_3D('',#11067,#8669,#8670);
#7314=AXIS2_PLACEMENT_3D('',#11069,#8672,#8673);
#7315=AXIS2_PLACEMENT_3D('',#11071,#8674,#8675);
#7316=AXIS2_PLACEMENT_3D('',#11073,#8677,#8678);
#7317=AXIS2_PLACEMENT_3D('',#11075,#8679,#8680);
#7318=AXIS2_PLACEMENT_3D('',#11077,#8682,#8683);
#7319=AXIS2_PLACEMENT_3D('',#11078,#8684,#8685);
#7320=AXIS2_PLACEMENT_3D('',#11087,#8690,#8691);
#7321=AXIS2_PLACEMENT_3D('',#11093,#8695,#8696);
#7322=AXIS2_PLACEMENT_3D('',#11099,#8700,#8701);
#7323=AXIS2_PLACEMENT_3D('',#11105,#8705,#8706);
#7324=AXIS2_PLACEMENT_3D('',#11111,#8710,#8711);
#7325=AXIS2_PLACEMENT_3D('',#11114,#8714,#8715);
#7326=AXIS2_PLACEMENT_3D('',#11115,#8716,#8717);
#7327=AXIS2_PLACEMENT_3D('',#11116,#8718,#8719);
#7328=AXIS2_PLACEMENT_3D('',#11117,#8720,#8721);
#7329=AXIS2_PLACEMENT_3D('',#11119,#8722,#8723);
#7330=AXIS2_PLACEMENT_3D('',#11120,#8724,#8725);
#7331=AXIS2_PLACEMENT_3D('',#11122,#8726,#8727);
#7332=AXIS2_PLACEMENT_3D('',#11124,#8729,#8730);
#7333=AXIS2_PLACEMENT_3D('',#11126,#8731,#8732);
#7334=AXIS2_PLACEMENT_3D('',#11128,#8734,#8735);
#7335=AXIS2_PLACEMENT_3D('',#11130,#8736,#8737);
#7336=AXIS2_PLACEMENT_3D('',#11132,#8739,#8740);
#7337=AXIS2_PLACEMENT_3D('',#11134,#8741,#8742);
#7338=AXIS2_PLACEMENT_3D('',#11135,#8743,#8744);
#7339=AXIS2_PLACEMENT_3D('',#11137,#8745,#8746);
#7340=AXIS2_PLACEMENT_3D('',#11139,#8748,#8749);
#7341=AXIS2_PLACEMENT_3D('',#11141,#8750,#8751);
#7342=AXIS2_PLACEMENT_3D('',#11143,#8753,#8754);
#7343=AXIS2_PLACEMENT_3D('',#11145,#8755,#8756);
#7344=AXIS2_PLACEMENT_3D('',#11147,#8758,#8759);
#7345=AXIS2_PLACEMENT_3D('',#11148,#8760,#8761);
#7346=AXIS2_PLACEMENT_3D('',#11157,#8766,#8767);
#7347=AXIS2_PLACEMENT_3D('',#11163,#8771,#8772);
#7348=AXIS2_PLACEMENT_3D('',#11169,#8776,#8777);
#7349=AXIS2_PLACEMENT_3D('',#11175,#8781,#8782);
#7350=AXIS2_PLACEMENT_3D('',#11181,#8786,#8787);
#7351=AXIS2_PLACEMENT_3D('',#11184,#8790,#8791);
#7352=AXIS2_PLACEMENT_3D('',#11185,#8792,#8793);
#7353=AXIS2_PLACEMENT_3D('',#11186,#8794,#8795);
#7354=AXIS2_PLACEMENT_3D('',#11187,#8796,#8797);
#7355=AXIS2_PLACEMENT_3D('',#11188,#8798,#8799);
#7356=AXIS2_PLACEMENT_3D('',#11189,#8800,#8801);
#7357=AXIS2_PLACEMENT_3D('',#11190,#8802,#8803);
#7358=AXIS2_PLACEMENT_3D('',#11191,#8804,#8805);
#7359=AXIS2_PLACEMENT_3D('',#11192,#8806,#8807);
#7360=AXIS2_PLACEMENT_3D('',#11193,#8808,#8809);
#7361=AXIS2_PLACEMENT_3D('',#11194,#8810,#8811);
#7362=AXIS2_PLACEMENT_3D('',#11195,#8812,#8813);
#7363=AXIS2_PLACEMENT_3D('',#11196,#8814,#8815);
#7364=AXIS2_PLACEMENT_3D('',#11197,#8816,#8817);
#7365=AXIS2_PLACEMENT_3D('',#11198,#8818,#8819);
#7366=AXIS2_PLACEMENT_3D('',#11199,#8820,#8821);
#7367=AXIS2_PLACEMENT_3D('',#11200,#8822,#8823);
#7368=AXIS2_PLACEMENT_3D('',#11201,#8824,#8825);
#7369=AXIS2_PLACEMENT_3D('',#11202,#8826,#8827);
#7370=AXIS2_PLACEMENT_3D('',#11203,#8828,#8829);
#7371=AXIS2_PLACEMENT_3D('',#11204,#8830,#8831);
#7372=AXIS2_PLACEMENT_3D('',#11205,#8832,#8833);
#7373=AXIS2_PLACEMENT_3D('',#11206,#8834,#8835);
#7374=AXIS2_PLACEMENT_3D('',#11207,#8836,#8837);
#7375=AXIS2_PLACEMENT_3D('',#11208,#8838,#8839);
#7376=AXIS2_PLACEMENT_3D('',#11209,#8840,#8841);
#7377=AXIS2_PLACEMENT_3D('',#11218,#8846,#8847);
#7378=AXIS2_PLACEMENT_3D('',#11220,#8848,#8849);
#7379=AXIS2_PLACEMENT_3D('',#11224,#8852,#8853);
#7380=AXIS2_PLACEMENT_3D('',#11230,#8857,#8858);
#7381=AXIS2_PLACEMENT_3D('',#11232,#8860,#8861);
#7382=AXIS2_PLACEMENT_3D('',#11233,#8862,#8863);
#7383=AXIS2_PLACEMENT_3D('',#11234,#8864,#8865);
#7384=AXIS2_PLACEMENT_3D('',#11243,#8870,#8871);
#7385=AXIS2_PLACEMENT_3D('',#11245,#8872,#8873);
#7386=AXIS2_PLACEMENT_3D('',#11249,#8876,#8877);
#7387=AXIS2_PLACEMENT_3D('',#11255,#8881,#8882);
#7388=AXIS2_PLACEMENT_3D('',#11257,#8884,#8885);
#7389=AXIS2_PLACEMENT_3D('',#11258,#8886,#8887);
#7390=AXIS2_PLACEMENT_3D('',#11259,#8888,#8889);
#7391=AXIS2_PLACEMENT_3D('',#11261,#8890,#8891);
#7392=AXIS2_PLACEMENT_3D('',#11263,#8892,#8893);
#7393=AXIS2_PLACEMENT_3D('',#11264,#8894,#8895);
#7394=AXIS2_PLACEMENT_3D('',#11266,#8896,#8897);
#7395=AXIS2_PLACEMENT_3D('',#11268,#8898,#8899);
#7396=AXIS2_PLACEMENT_3D('',#11269,#8900,#8901);
#7397=AXIS2_PLACEMENT_3D('',#11271,#8903,#8904);
#7398=AXIS2_PLACEMENT_3D('',#11274,#8906,#8907);
#7399=AXIS2_PLACEMENT_3D('',#11275,#8908,#8909);
#7400=AXIS2_PLACEMENT_3D('',#11277,#8910,#8911);
#7401=AXIS2_PLACEMENT_3D('',#11279,#8913,#8914);
#7402=AXIS2_PLACEMENT_3D('',#11280,#8915,#8916);
#7403=AXIS2_PLACEMENT_3D('',#11281,#8917,#8918);
#7404=AXIS2_PLACEMENT_3D('',#11282,#8919,#8920);
#7405=AXIS2_PLACEMENT_3D('',#11284,#8921,#8922);
#7406=AXIS2_PLACEMENT_3D('',#11287,#8924,#8925);
#7407=AXIS2_PLACEMENT_3D('',#11288,#8926,#8927);
#7408=AXIS2_PLACEMENT_3D('',#11290,#8928,#8929);
#7409=AXIS2_PLACEMENT_3D('',#11293,#8931,#8932);
#7410=AXIS2_PLACEMENT_3D('',#11294,#8933,#8934);
#7411=AXIS2_PLACEMENT_3D('',#11295,#8935,#8936);
#7412=AXIS2_PLACEMENT_3D('',#11296,#8937,#8938);
#7413=AXIS2_PLACEMENT_3D('',#11297,#8939,#8940);
#7414=AXIS2_PLACEMENT_3D('',#11301,#8942,#8943);
#7415=AXIS2_PLACEMENT_3D('',#11302,#8944,#8945);
#7416=AXIS2_PLACEMENT_3D('',#11319,#8946,#8947);
#7417=AXIS2_PLACEMENT_3D('',#11360,#8949,#8950);
#7418=AXIS2_PLACEMENT_3D('',#11375,#8951,#8952);
#7419=AXIS2_PLACEMENT_3D('',#11377,#8954,#8955);
#7420=AXIS2_PLACEMENT_3D('',#11379,#8956,#8957);
#7421=AXIS2_PLACEMENT_3D('',#11382,#8959,#8960);
#7422=AXIS2_PLACEMENT_3D('',#11383,#8961,#8962);
#7423=AXIS2_PLACEMENT_3D('',#11385,#8963,#8964);
#7424=AXIS2_PLACEMENT_3D('',#11388,#8966,#8967);
#7425=AXIS2_PLACEMENT_3D('',#11389,#8968,#8969);
#7426=AXIS2_PLACEMENT_3D('',#11390,#8970,#8971);
#7427=AXIS2_PLACEMENT_3D('',#11391,#8972,#8973);
#7428=AXIS2_PLACEMENT_3D('',#11392,#8974,#8975);
#7429=AXIS2_PLACEMENT_3D('',#11396,#8977,#8978);
#7430=AXIS2_PLACEMENT_3D('',#11397,#8979,#8980);
#7431=AXIS2_PLACEMENT_3D('',#11414,#8981,#8982);
#7432=AXIS2_PLACEMENT_3D('',#11455,#8984,#8985);
#7433=AXIS2_PLACEMENT_3D('',#11470,#8986,#8987);
#7434=AXIS2_PLACEMENT_3D('',#11472,#8989,#8990);
#7435=AXIS2_PLACEMENT_3D('',#11481,#8995,#8996);
#7436=AXIS2_PLACEMENT_3D('',#11491,#9002,#9003);
#7437=AXIS2_PLACEMENT_3D('',#11501,#9009,#9010);
#7438=AXIS2_PLACEMENT_3D('',#11504,#9013,#9014);
#7439=AXIS2_PLACEMENT_3D('',#11505,#9015,#9016);
#7440=AXIS2_PLACEMENT_3D('',#11507,#9017,#9018);
#7441=AXIS2_PLACEMENT_3D('',#11508,#9019,#9020);
#7442=AXIS2_PLACEMENT_3D('',#11509,#9021,#9022);
#7443=AXIS2_PLACEMENT_3D('',#11518,#9027,#9028);
#7444=AXIS2_PLACEMENT_3D('',#11524,#9032,#9033);
#7445=AXIS2_PLACEMENT_3D('',#11530,#9037,#9038);
#7446=AXIS2_PLACEMENT_3D('',#11533,#9041,#9042);
#7447=AXIS2_PLACEMENT_3D('',#11534,#9043,#9044);
#7448=AXIS2_PLACEMENT_3D('',#11535,#9045,#9046);
#7449=AXIS2_PLACEMENT_3D('',#11536,#9047,#9048);
#7450=AXIS2_PLACEMENT_3D('',#11538,#9049,#9050);
#7451=AXIS2_PLACEMENT_3D('',#11539,#9051,#9052);
#7452=AXIS2_PLACEMENT_3D('',#11540,#9053,#9054);
#7453=AXIS2_PLACEMENT_3D('',#11542,#9056,#9057);
#7454=AXIS2_PLACEMENT_3D('',#11543,#9058,#9059);
#7455=AXIS2_PLACEMENT_3D('',#11547,#9061,#9062);
#7456=AXIS2_PLACEMENT_3D('',#11548,#9063,#9064);
#7457=AXIS2_PLACEMENT_3D('',#11565,#9065,#9066);
#7458=AXIS2_PLACEMENT_3D('',#11606,#9068,#9069);
#7459=AXIS2_PLACEMENT_3D('',#11621,#9070,#9071);
#7460=AXIS2_PLACEMENT_3D('',#11623,#9073,#9074);
#7461=AXIS2_PLACEMENT_3D('',#11632,#9079,#9080);
#7462=AXIS2_PLACEMENT_3D('',#11638,#9084,#9085);
#7463=AXIS2_PLACEMENT_3D('',#11644,#9089,#9090);
#7464=AXIS2_PLACEMENT_3D('',#11646,#9091,#9092);
#7465=AXIS2_PLACEMENT_3D('',#11647,#9093,#9094);
#7466=AXIS2_PLACEMENT_3D('',#11648,#9095,#9096);
#7467=AXIS2_PLACEMENT_3D('',#11649,#9097,#9098);
#7468=AXIS2_PLACEMENT_3D('',#11650,#9099,#9100);
#7469=AXIS2_PLACEMENT_3D('',#11652,#9101,#9102);
#7470=AXIS2_PLACEMENT_3D('',#11655,#9104,#9105);
#7471=AXIS2_PLACEMENT_3D('',#11656,#9106,#9107);
#7472=AXIS2_PLACEMENT_3D('',#11661,#9109,#9110);
#7473=AXIS2_PLACEMENT_3D('',#11664,#9112,#9113);
#7474=AXIS2_PLACEMENT_3D('',#11665,#9114,#9115);
#7475=AXIS2_PLACEMENT_3D('',#11669,#9117,#9118);
#7476=AXIS2_PLACEMENT_3D('',#11671,#9120,#9121);
#7477=AXIS2_PLACEMENT_3D('',#11675,#9124,#9125);
#7478=AXIS2_PLACEMENT_3D('',#11678,#9127,#9128);
#7479=AXIS2_PLACEMENT_3D('',#11679,#9129,#9130);
#7480=AXIS2_PLACEMENT_3D('',#11681,#9132,#9133);
#7481=AXIS2_PLACEMENT_3D('',#11684,#9135,#9136);
#7482=AXIS2_PLACEMENT_3D('',#11685,#9137,#9138);
#7483=AXIS2_PLACEMENT_3D('',#11686,#9139,#9140);
#7484=AXIS2_PLACEMENT_3D('',#11687,#9141,#9142);
#7485=AXIS2_PLACEMENT_3D('',#11689,#9143,#9144);
#7486=AXIS2_PLACEMENT_3D('',#11692,#9146,#9147);
#7487=AXIS2_PLACEMENT_3D('',#11693,#9148,#9149);
#7488=AXIS2_PLACEMENT_3D('',#11695,#9150,#9151);
#7489=AXIS2_PLACEMENT_3D('',#11696,#9152,#9153);
#7490=AXIS2_PLACEMENT_3D('',#11699,#9155,#9156);
#7491=AXIS2_PLACEMENT_3D('',#11700,#9157,#9158);
#7492=AXIS2_PLACEMENT_3D('',#11702,#9159,#9160);
#7493=AXIS2_PLACEMENT_3D('',#11705,#9162,#9163);
#7494=AXIS2_PLACEMENT_3D('',#11706,#9164,#9165);
#7495=AXIS2_PLACEMENT_3D('',#11707,#9166,#9167);
#7496=AXIS2_PLACEMENT_3D('',#11708,#9168,#9169);
#7497=AXIS2_PLACEMENT_3D('',#11709,#9170,#9171);
#7498=AXIS2_PLACEMENT_3D('',#11711,#9172,#9173);
#7499=AXIS2_PLACEMENT_3D('',#11714,#9175,#9176);
#7500=AXIS2_PLACEMENT_3D('',#11715,#9177,#9178);
#7501=AXIS2_PLACEMENT_3D('',#11717,#9179,#9180);
#7502=AXIS2_PLACEMENT_3D('',#11718,#9181,#9182);
#7503=AXIS2_PLACEMENT_3D('',#11720,#9183,#9184);
#7504=AXIS2_PLACEMENT_3D('',#11722,#9186,#9187);
#7505=AXIS2_PLACEMENT_3D('',#11724,#9188,#9189);
#7506=AXIS2_PLACEMENT_3D('',#11727,#9191,#9192);
#7507=AXIS2_PLACEMENT_3D('',#11728,#9193,#9194);
#7508=AXIS2_PLACEMENT_3D('',#11729,#9195,#9196);
#7509=AXIS2_PLACEMENT_3D('',#11730,#9197,#9198);
#7510=AXIS2_PLACEMENT_3D('',#11731,#9199,#9200);
#7511=AXIS2_PLACEMENT_3D('',#11748,#9209,#9210);
#7512=AXIS2_PLACEMENT_3D('',#11754,#9214,#9215);
#7513=AXIS2_PLACEMENT_3D('',#11758,#9218,#9219);
#7514=AXIS2_PLACEMENT_3D('',#11762,#9222,#9223);
#7515=AXIS2_PLACEMENT_3D('',#11766,#9226,#9227);
#7516=AXIS2_PLACEMENT_3D('',#11774,#9232,#9233);
#7517=AXIS2_PLACEMENT_3D('',#11776,#9235,#9236);
#7518=AXIS2_PLACEMENT_3D('',#11778,#9238,#9239);
#7519=AXIS2_PLACEMENT_3D('',#11780,#9241,#9242);
#7520=AXIS2_PLACEMENT_3D('',#11781,#9243,#9244);
#7521=AXIS2_PLACEMENT_3D('',#11782,#9245,#9246);
#7522=AXIS2_PLACEMENT_3D('',#11791,#9251,#9252);
#7523=AXIS2_PLACEMENT_3D('',#11797,#9256,#9257);
#7524=AXIS2_PLACEMENT_3D('',#11803,#9261,#9262);
#7525=AXIS2_PLACEMENT_3D('',#11809,#9266,#9267);
#7526=AXIS2_PLACEMENT_3D('',#11815,#9271,#9272);
#7527=AXIS2_PLACEMENT_3D('',#11818,#9275,#9276);
#7528=AXIS2_PLACEMENT_3D('',#11819,#9277,#9278);
#7529=AXIS2_PLACEMENT_3D('',#11821,#9279,#9280);
#7530=AXIS2_PLACEMENT_3D('',#11822,#9281,#9282);
#7531=AXIS2_PLACEMENT_3D('',#11824,#9283,#9284);
#7532=AXIS2_PLACEMENT_3D('',#11826,#9286,#9287);
#7533=AXIS2_PLACEMENT_3D('',#11828,#9288,#9289);
#7534=AXIS2_PLACEMENT_3D('',#11830,#9291,#9292);
#7535=AXIS2_PLACEMENT_3D('',#11832,#9293,#9294);
#7536=AXIS2_PLACEMENT_3D('',#11834,#9296,#9297);
#7537=AXIS2_PLACEMENT_3D('',#11835,#9298,#9299);
#7538=AXIS2_PLACEMENT_3D('',#11836,#9300,#9301);
#7539=AXIS2_PLACEMENT_3D('',#11837,#9302,#9303);
#7540=AXIS2_PLACEMENT_3D('',#11840,#9304,#9305);
#7541=AXIS2_PLACEMENT_3D('',#11841,#9306,#9307);
#7542=AXIS2_PLACEMENT_3D('',#11843,#9308,#9309);
#7543=AXIS2_PLACEMENT_3D('',#11845,#9310,#9311);
#7544=AXIS2_PLACEMENT_3D('',#11846,#9312,#9313);
#7545=AXIS2_PLACEMENT_3D('',#11847,#9314,#9315);
#7546=AXIS2_PLACEMENT_3D('',#11850,#9317,#9318);
#7547=AXIS2_PLACEMENT_3D('',#11851,#9319,#9320);
#7548=AXIS2_PLACEMENT_3D('',#11853,#9321,#9322);
#7549=AXIS2_PLACEMENT_3D('',#11856,#9324,#9325);
#7550=AXIS2_PLACEMENT_3D('',#11857,#9326,#9327);
#7551=AXIS2_PLACEMENT_3D('',#11860,#9329,#9330);
#7552=AXIS2_PLACEMENT_3D('',#11861,#9331,#9332);
#7553=AXIS2_PLACEMENT_3D('',#11862,#9333,#9334);
#7554=AXIS2_PLACEMENT_3D('',#11864,#9335,#9336);
#7555=AXIS2_PLACEMENT_3D('',#11866,#9338,#9339);
#7556=AXIS2_PLACEMENT_3D('',#11868,#9340,#9341);
#7557=AXIS2_PLACEMENT_3D('',#11869,#9342,#9343);
#7558=AXIS2_PLACEMENT_3D('',#11871,#9345,#9346);
#7559=AXIS2_PLACEMENT_3D('',#11872,#9347,#9348);
#7560=AXIS2_PLACEMENT_3D('',#11875,#9349,#9350);
#7561=AXIS2_PLACEMENT_3D('',#11876,#9351,#9352);
#7562=AXIS2_PLACEMENT_3D('',#11878,#9353,#9354);
#7563=AXIS2_PLACEMENT_3D('',#11880,#9355,#9356);
#7564=AXIS2_PLACEMENT_3D('',#11881,#9357,#9358);
#7565=AXIS2_PLACEMENT_3D('',#11882,#9359,#9360);
#7566=AXIS2_PLACEMENT_3D('',#11884,#9361,#9362);
#7567=AXIS2_PLACEMENT_3D('',#11886,#9364,#9365);
#7568=AXIS2_PLACEMENT_3D('',#11888,#9366,#9367);
#7569=AXIS2_PLACEMENT_3D('',#11890,#9368,#9369);
#7570=AXIS2_PLACEMENT_3D('',#11891,#9370,#9371);
#7571=AXIS2_PLACEMENT_3D('',#11893,#9372,#9373);
#7572=AXIS2_PLACEMENT_3D('',#11895,#9375,#9376);
#7573=AXIS2_PLACEMENT_3D('',#11897,#9377,#9378);
#7574=AXIS2_PLACEMENT_3D('',#11899,#9380,#9381);
#7575=AXIS2_PLACEMENT_3D('',#11901,#9382,#9383);
#7576=AXIS2_PLACEMENT_3D('',#11903,#9385,#9386);
#7577=AXIS2_PLACEMENT_3D('',#11904,#9387,#9388);
#7578=AXIS2_PLACEMENT_3D('',#11906,#9390,#9391);
#7579=AXIS2_PLACEMENT_3D('',#11907,#9392,#9393);
#7580=AXIS2_PLACEMENT_3D('',#11910,#9394,#9395);
#7581=AXIS2_PLACEMENT_3D('',#11911,#9396,#9397);
#7582=AXIS2_PLACEMENT_3D('',#11914,#9398,#9399);
#7583=AXIS2_PLACEMENT_3D('',#11915,#9400,#9401);
#7584=AXIS2_PLACEMENT_3D('',#11918,#9402,#9403);
#7585=AXIS2_PLACEMENT_3D('',#11919,#9404,#9405);
#7586=AXIS2_PLACEMENT_3D('',#11922,#9406,#9407);
#7587=AXIS2_PLACEMENT_3D('',#11923,#9408,#9409);
#7588=AXIS2_PLACEMENT_3D('',#11926,#9410,#9411);
#7589=AXIS2_PLACEMENT_3D('',#11927,#9412,#9413);
#7590=AXIS2_PLACEMENT_3D('',#11930,#9414,#9415);
#7591=AXIS2_PLACEMENT_3D('',#11931,#9416,#9417);
#7592=AXIS2_PLACEMENT_3D('',#11934,#9418,#9419);
#7593=AXIS2_PLACEMENT_3D('',#11935,#9420,#9421);
#7594=AXIS2_PLACEMENT_3D('',#11938,#9422,#9423);
#7595=AXIS2_PLACEMENT_3D('',#11939,#9424,#9425);
#7596=AXIS2_PLACEMENT_3D('',#11940,#9426,#9427);
#7597=AXIS2_PLACEMENT_3D('',#11966,#9428,#9429);
#7598=AXIS2_PLACEMENT_3D('',#11990,#9430,#9431);
#7599=AXIS2_PLACEMENT_3D('',#11991,#9432,#9433);
#7600=AXIS2_PLACEMENT_3D('',#11993,#9434,#9435);
#7601=AXIS2_PLACEMENT_3D('',#12018,#9436,#9437);
#7602=AXIS2_PLACEMENT_3D('',#12043,#9438,#9439);
#7603=AXIS2_PLACEMENT_3D('',#12059,#9441,#9442);
#7604=AXIS2_PLACEMENT_3D('',#12074,#9443,#9444);
#7605=AXIS2_PLACEMENT_3D('',#12099,#9445,#9446);
#7606=AXIS2_PLACEMENT_3D('',#12124,#9447,#9448);
#7607=AXIS2_PLACEMENT_3D('',#12149,#9449,#9450);
#7608=AXIS2_PLACEMENT_3D('',#12173,#9451,#9452);
#7609=AXIS2_PLACEMENT_3D('',#12174,#9453,#9454);
#7610=AXIS2_PLACEMENT_3D('',#12176,#9455,#9456);
#7611=AXIS2_PLACEMENT_3D('',#12177,#9457,#9458);
#7612=AXIS2_PLACEMENT_3D('',#12178,#9459,#9460);
#7613=AXIS2_PLACEMENT_3D('',#12202,#9461,#9462);
#7614=AXIS2_PLACEMENT_3D('',#12203,#9463,#9464);
#7615=AXIS2_PLACEMENT_3D('',#12205,#9465,#9466);
#7616=AXIS2_PLACEMENT_3D('',#12206,#9467,#9468);
#7617=AXIS2_PLACEMENT_3D('',#12207,#9469,#9470);
#7618=AXIS2_PLACEMENT_3D('',#12231,#9471,#9472);
#7619=AXIS2_PLACEMENT_3D('',#12232,#9473,#9474);
#7620=AXIS2_PLACEMENT_3D('',#12234,#9475,#9476);
#7621=AXIS2_PLACEMENT_3D('',#12235,#9477,#9478);
#7622=AXIS2_PLACEMENT_3D('',#12236,#9479,#9480);
#7623=AXIS2_PLACEMENT_3D('',#12251,#9481,#9482);
#7624=AXIS2_PLACEMENT_3D('',#12264,#9483,#9484);
#7625=AXIS2_PLACEMENT_3D('',#12266,#9485,#9486);
#7626=AXIS2_PLACEMENT_3D('',#12267,#9487,#9488);
#7627=AXIS2_PLACEMENT_3D('',#12268,#9489,#9490);
#7628=AXIS2_PLACEMENT_3D('',#12292,#9491,#9492);
#7629=AXIS2_PLACEMENT_3D('',#12293,#9493,#9494);
#7630=AXIS2_PLACEMENT_3D('',#12295,#9495,#9496);
#7631=AXIS2_PLACEMENT_3D('',#12296,#9497,#9498);
#7632=AXIS2_PLACEMENT_3D('',#12297,#9499,#9500);
#7633=AXIS2_PLACEMENT_3D('',#12321,#9501,#9502);
#7634=AXIS2_PLACEMENT_3D('',#12322,#9503,#9504);
#7635=AXIS2_PLACEMENT_3D('',#12324,#9505,#9506);
#7636=AXIS2_PLACEMENT_3D('',#12325,#9507,#9508);
#7637=AXIS2_PLACEMENT_3D('',#12326,#9509,#9510);
#7638=AXIS2_PLACEMENT_3D('',#12350,#9511,#9512);
#7639=AXIS2_PLACEMENT_3D('',#12351,#9513,#9514);
#7640=AXIS2_PLACEMENT_3D('',#12353,#9515,#9516);
#7641=AXIS2_PLACEMENT_3D('',#12356,#9518,#9519);
#7642=AXIS2_PLACEMENT_3D('',#12380,#9520,#9521);
#7643=AXIS2_PLACEMENT_3D('',#12381,#9522,#9523);
#7644=AXIS2_PLACEMENT_3D('',#12382,#9524,#9525);
#7645=AXIS2_PLACEMENT_3D('',#12383,#9526,#9527);
#7646=AXIS2_PLACEMENT_3D('',#12384,#9528,#9529);
#7647=AXIS2_PLACEMENT_3D('',#12385,#9530,#9531);
#7648=AXIS2_PLACEMENT_3D('',#12386,#9532,#9533);
#7649=AXIS2_PLACEMENT_3D('',#12387,#9534,#9535);
#7650=AXIS2_PLACEMENT_3D('',#12388,#9536,#9537);
#7651=AXIS2_PLACEMENT_3D('',#12390,#9538,#9539);
#7652=AXIS2_PLACEMENT_3D('',#12392,#9540,#9541);
#7653=AXIS2_PLACEMENT_3D('',#12393,#9542,#9543);
#7654=AXIS2_PLACEMENT_3D('',#12395,#9544,#9545);
#7655=AXIS2_PLACEMENT_3D('',#12397,#9547,#9548);
#7656=AXIS2_PLACEMENT_3D('',#12399,#9549,#9550);
#7657=AXIS2_PLACEMENT_3D('',#12400,#9551,#9552);
#7658=AXIS2_PLACEMENT_3D('',#12402,#9554,#9555);
#7659=AXIS2_PLACEMENT_3D('',#12404,#9556,#9557);
#7660=AXIS2_PLACEMENT_3D('',#12406,#9558,#9559);
#7661=AXIS2_PLACEMENT_3D('',#12407,#9560,#9561);
#7662=AXIS2_PLACEMENT_3D('',#12409,#9562,#9563);
#7663=AXIS2_PLACEMENT_3D('',#12411,#9565,#9566);
#7664=AXIS2_PLACEMENT_3D('',#12413,#9567,#9568);
#7665=AXIS2_PLACEMENT_3D('',#12414,#9569,#9570);
#7666=AXIS2_PLACEMENT_3D('',#12416,#9572,#9573);
#7667=AXIS2_PLACEMENT_3D('',#12417,#9574,#9575);
#7668=AXIS2_PLACEMENT_3D('',#12418,#9576,#9577);
#7669=AXIS2_PLACEMENT_3D('',#12419,#9578,#9579);
#7670=AXIS2_PLACEMENT_3D('',#12420,#9580,#9581);
#7671=AXIS2_PLACEMENT_3D('',#12421,#9582,#9583);
#7672=AXIS2_PLACEMENT_3D('',#12422,#9584,#9585);
#7673=AXIS2_PLACEMENT_3D('',#12423,#9586,#9587);
#7674=AXIS2_PLACEMENT_3D('',#12424,#9588,#9589);
#7675=AXIS2_PLACEMENT_3D('',#12425,#9590,#9591);
#7676=AXIS2_PLACEMENT_3D('',#12426,#9592,#9593);
#7677=AXIS2_PLACEMENT_3D('',#12427,#9594,#9595);
#7678=AXIS2_PLACEMENT_3D('',#12428,#9596,#9597);
#7679=AXIS2_PLACEMENT_3D('',#12429,#9598,#9599);
#7680=AXIS2_PLACEMENT_3D('',#12430,#9600,#9601);
#7681=AXIS2_PLACEMENT_3D('',#12431,#9602,#9603);
#7682=AXIS2_PLACEMENT_3D('',#12432,#9604,#9605);
#7683=AXIS2_PLACEMENT_3D('',#12433,#9606,#9607);
#7684=AXIS2_PLACEMENT_3D('',#12434,#9608,#9609);
#7685=AXIS2_PLACEMENT_3D('',#12435,#9610,#9611);
#7686=AXIS2_PLACEMENT_3D('',#12436,#9612,#9613);
#7687=AXIS2_PLACEMENT_3D('',#12438,#9614,#9615);
#7688=AXIS2_PLACEMENT_3D('',#12441,#9617,#9618);
#7689=AXIS2_PLACEMENT_3D('',#12442,#9619,#9620);
#7690=AXIS2_PLACEMENT_3D('',#12444,#9621,#9622);
#7691=AXIS2_PLACEMENT_3D('',#12447,#9624,#9625);
#7692=AXIS2_PLACEMENT_3D('',#12448,#9626,#9627);
#7693=AXIS2_PLACEMENT_3D('',#12450,#9628,#9629);
#7694=AXIS2_PLACEMENT_3D('',#12453,#9631,#9632);
#7695=AXIS2_PLACEMENT_3D('',#12454,#9633,#9634);
#7696=AXIS2_PLACEMENT_3D('',#12463,#9639,#9640);
#7697=AXIS2_PLACEMENT_3D('',#12472,#9645,#9646);
#7698=AXIS2_PLACEMENT_3D('',#12478,#9650,#9651);
#7699=AXIS2_PLACEMENT_3D('',#12481,#9654,#9655);
#7700=AXIS2_PLACEMENT_3D('',#12487,#9659,#9660);
#7701=AXIS2_PLACEMENT_3D('',#12493,#9664,#9665);
#7702=AXIS2_PLACEMENT_3D('',#12497,#9668,#9669);
#7703=AXIS2_PLACEMENT_3D('',#12501,#9672,#9673);
#7704=AXIS2_PLACEMENT_3D('',#12503,#9675,#9676);
#7705=AXIS2_PLACEMENT_3D('',#12504,#9677,#9678);
#7706=AXIS2_PLACEMENT_3D('',#12505,#9679,#9680);
#7707=AXIS2_PLACEMENT_3D('',#12507,#9681,#9682);
#7708=AXIS2_PLACEMENT_3D('',#12510,#9684,#9685);
#7709=AXIS2_PLACEMENT_3D('',#12511,#9686,#9687);
#7710=AXIS2_PLACEMENT_3D('',#12512,#9688,#9689);
#7711=AXIS2_PLACEMENT_3D('',#12514,#9690,#9691);
#7712=AXIS2_PLACEMENT_3D('',#12517,#9693,#9694);
#7713=AXIS2_PLACEMENT_3D('',#12518,#9695,#9696);
#7714=AXIS2_PLACEMENT_3D('',#12519,#9697,#9698);
#7715=AXIS2_PLACEMENT_3D('',#12521,#9699,#9700);
#7716=AXIS2_PLACEMENT_3D('',#12524,#9702,#9703);
#7717=AXIS2_PLACEMENT_3D('',#12525,#9704,#9705);
#7718=AXIS2_PLACEMENT_3D('',#12526,#9706,#9707);
#7719=AXIS2_PLACEMENT_3D('',#12527,#9708,#9709);
#7720=AXIS2_PLACEMENT_3D('',#12528,#9710,#9711);
#7721=AXIS2_PLACEMENT_3D('',#12530,#9712,#9713);
#7722=AXIS2_PLACEMENT_3D('',#12533,#9715,#9716);
#7723=AXIS2_PLACEMENT_3D('',#12534,#9717,#9718);
#7724=AXIS2_PLACEMENT_3D('',#12536,#9719,#9720);
#7725=AXIS2_PLACEMENT_3D('',#12539,#9722,#9723);
#7726=AXIS2_PLACEMENT_3D('',#12540,#9724,#9725);
#7727=AXIS2_PLACEMENT_3D('',#12541,#9726,#9727);
#7728=AXIS2_PLACEMENT_3D('',#12542,#9728,#9729);
#7729=AXIS2_PLACEMENT_3D('',#12543,#9730,#9731);
#7730=AXIS2_PLACEMENT_3D('',#12545,#9732,#9733);
#7731=AXIS2_PLACEMENT_3D('',#12548,#9735,#9736);
#7732=AXIS2_PLACEMENT_3D('',#12549,#9737,#9738);
#7733=AXIS2_PLACEMENT_3D('',#12551,#9739,#9740);
#7734=AXIS2_PLACEMENT_3D('',#12554,#9742,#9743);
#7735=AXIS2_PLACEMENT_3D('',#12555,#9744,#9745);
#7736=AXIS2_PLACEMENT_3D('',#12556,#9746,#9747);
#7737=AXIS2_PLACEMENT_3D('',#12557,#9748,#9749);
#7738=AXIS2_PLACEMENT_3D('',#12558,#9750,#9751);
#7739=AXIS2_PLACEMENT_3D('',#12560,#9752,#9753);
#7740=AXIS2_PLACEMENT_3D('',#12563,#9755,#9756);
#7741=AXIS2_PLACEMENT_3D('',#12564,#9757,#9758);
#7742=AXIS2_PLACEMENT_3D('',#12566,#9759,#9760);
#7743=AXIS2_PLACEMENT_3D('',#12569,#9762,#9763);
#7744=AXIS2_PLACEMENT_3D('',#12570,#9764,#9765);
#7745=AXIS2_PLACEMENT_3D('',#12571,#9766,#9767);
#7746=AXIS2_PLACEMENT_3D('',#12572,#9768,#9769);
#7747=AXIS2_PLACEMENT_3D('',#12573,#9770,#9771);
#7748=AXIS2_PLACEMENT_3D('',#12575,#9772,#9773);
#7749=AXIS2_PLACEMENT_3D('',#12578,#9775,#9776);
#7750=AXIS2_PLACEMENT_3D('',#12579,#9777,#9778);
#7751=AXIS2_PLACEMENT_3D('',#12581,#9779,#9780);
#7752=AXIS2_PLACEMENT_3D('',#12584,#9782,#9783);
#7753=AXIS2_PLACEMENT_3D('',#12585,#9784,#9785);
#7754=AXIS2_PLACEMENT_3D('',#12586,#9786,#9787);
#7755=AXIS2_PLACEMENT_3D('',#12587,#9788,#9789);
#7756=AXIS2_PLACEMENT_3D('',#12588,#9790,#9791);
#7757=AXIS2_PLACEMENT_3D('',#12590,#9792,#9793);
#7758=AXIS2_PLACEMENT_3D('',#12593,#9795,#9796);
#7759=AXIS2_PLACEMENT_3D('',#12594,#9797,#9798);
#7760=AXIS2_PLACEMENT_3D('',#12596,#9799,#9800);
#7761=AXIS2_PLACEMENT_3D('',#12599,#9802,#9803);
#7762=AXIS2_PLACEMENT_3D('',#12600,#9804,#9805);
#7763=AXIS2_PLACEMENT_3D('',#12601,#9806,#9807);
#7764=AXIS2_PLACEMENT_3D('',#12602,#9808,#9809);
#7765=AXIS2_PLACEMENT_3D('',#12603,#9810,#9811);
#7766=AXIS2_PLACEMENT_3D('',#12605,#9812,#9813);
#7767=AXIS2_PLACEMENT_3D('',#12608,#9815,#9816);
#7768=AXIS2_PLACEMENT_3D('',#12609,#9817,#9818);
#7769=AXIS2_PLACEMENT_3D('',#12611,#9819,#9820);
#7770=AXIS2_PLACEMENT_3D('',#12614,#9822,#9823);
#7771=AXIS2_PLACEMENT_3D('',#12615,#9824,#9825);
#7772=AXIS2_PLACEMENT_3D('',#12616,#9826,#9827);
#7773=AXIS2_PLACEMENT_3D('',#12617,#9828,#9829);
#7774=AXIS2_PLACEMENT_3D('',#12618,#9830,#9831);
#7775=AXIS2_PLACEMENT_3D('',#12627,#9836,#9837);
#7776=AXIS2_PLACEMENT_3D('',#12633,#9841,#9842);
#7777=AXIS2_PLACEMENT_3D('',#12639,#9846,#9847);
#7778=AXIS2_PLACEMENT_3D('',#12645,#9851,#9852);
#7779=AXIS2_PLACEMENT_3D('',#12651,#9856,#9857);
#7780=AXIS2_PLACEMENT_3D('',#12654,#9860,#9861);
#7781=AXIS2_PLACEMENT_3D('',#12655,#9862,#9863);
#7782=AXIS2_PLACEMENT_3D('',#12656,#9864,#9865);
#7783=AXIS2_PLACEMENT_3D('',#12658,#9866,#9867);
#7784=AXIS2_PLACEMENT_3D('',#12659,#9868,#9869);
#7785=AXIS2_PLACEMENT_3D('',#12661,#9870,#9871);
#7786=AXIS2_PLACEMENT_3D('',#12662,#9872,#9873);
#7787=AXIS2_PLACEMENT_3D('',#12664,#9874,#9875);
#7788=AXIS2_PLACEMENT_3D('',#12666,#9877,#9878);
#7789=AXIS2_PLACEMENT_3D('',#12668,#9879,#9880);
#7790=AXIS2_PLACEMENT_3D('',#12670,#9882,#9883);
#7791=AXIS2_PLACEMENT_3D('',#12672,#9884,#9885);
#7792=AXIS2_PLACEMENT_3D('',#12674,#9887,#9888);
#7793=AXIS2_PLACEMENT_3D('',#12676,#9889,#9890);
#7794=AXIS2_PLACEMENT_3D('',#12677,#9891,#9892);
#7795=AXIS2_PLACEMENT_3D('',#12679,#9893,#9894);
#7796=AXIS2_PLACEMENT_3D('',#12681,#9896,#9897);
#7797=AXIS2_PLACEMENT_3D('',#12683,#9899,#9900);
#7798=AXIS2_PLACEMENT_3D('',#12684,#9901,#9902);
#7799=AXIS2_PLACEMENT_3D('',#12685,#9903,#9904);
#7800=AXIS2_PLACEMENT_3D('',#12686,#9905,#9906);
#7801=AXIS2_PLACEMENT_3D('',#12687,#9907,#9908);
#7802=AXIS2_PLACEMENT_3D('',#12688,#9909,#9910);
#7803=AXIS2_PLACEMENT_3D('',#12689,#9911,#9912);
#7804=AXIS2_PLACEMENT_3D('',#12690,#9913,#9914);
#7805=AXIS2_PLACEMENT_3D('',#12691,#9915,#9916);
#7806=AXIS2_PLACEMENT_3D('',#12692,#9917,#9918);
#7807=AXIS2_PLACEMENT_3D('',#12693,#9919,#9920);
#7808=AXIS2_PLACEMENT_3D('',#12694,#9921,#9922);
#7809=AXIS2_PLACEMENT_3D('',#12695,#9923,#9924);
#7810=DIRECTION('axis',(0.,0.,1.));
#7811=DIRECTION('refdir',(1.,0.,0.));
#7812=DIRECTION('axis',(0.,0.,1.));
#7813=DIRECTION('refdir',(1.,0.,0.));
#7814=DIRECTION('axis',(0.,0.,1.));
#7815=DIRECTION('refdir',(1.,0.,0.));
#7816=DIRECTION('center_axis',(0.,0.,1.));
#7817=DIRECTION('ref_axis',(1.,0.,0.));
#7818=DIRECTION('center_axis',(0.,0.,1.));
#7819=DIRECTION('ref_axis',(1.,0.,0.));
#7820=DIRECTION('',(0.,0.,1.));
#7821=DIRECTION('center_axis',(0.,0.,-1.));
#7822=DIRECTION('ref_axis',(1.,0.,0.));
#7823=DIRECTION('center_axis',(0.,0.,1.));
#7824=DIRECTION('ref_axis',(1.,0.,0.));
#7825=DIRECTION('center_axis',(0.,0.,1.));
#7826=DIRECTION('ref_axis',(1.,0.,0.));
#7827=DIRECTION('',(0.,0.,1.));
#7828=DIRECTION('center_axis',(0.,0.,-1.));
#7829=DIRECTION('ref_axis',(1.,0.,0.));
#7830=DIRECTION('center_axis',(0.,0.,1.));
#7831=DIRECTION('ref_axis',(1.,0.,0.));
#7832=DIRECTION('center_axis',(0.,0.,1.));
#7833=DIRECTION('ref_axis',(1.,0.,0.));
#7834=DIRECTION('',(0.,0.,1.));
#7835=DIRECTION('center_axis',(0.,0.,-1.));
#7836=DIRECTION('ref_axis',(1.,0.,0.));
#7837=DIRECTION('center_axis',(0.,0.,1.));
#7838=DIRECTION('ref_axis',(1.,0.,0.));
#7839=DIRECTION('center_axis',(0.,0.,1.));
#7840=DIRECTION('ref_axis',(1.,0.,0.));
#7841=DIRECTION('',(0.,0.,1.));
#7842=DIRECTION('center_axis',(0.,0.,-1.));
#7843=DIRECTION('ref_axis',(1.,0.,0.));
#7844=DIRECTION('center_axis',(0.,1.,0.));
#7845=DIRECTION('ref_axis',(-1.,0.,0.));
#7846=DIRECTION('',(-1.,0.,0.));
#7847=DIRECTION('',(0.,0.,1.));
#7848=DIRECTION('',(-1.,0.,0.));
#7849=DIRECTION('',(0.,0.,1.));
#7850=DIRECTION('center_axis',(1.,0.,0.));
#7851=DIRECTION('ref_axis',(0.,1.,0.));
#7852=DIRECTION('',(0.,1.,0.));
#7853=DIRECTION('',(0.,1.,0.));
#7854=DIRECTION('',(0.,0.,1.));
#7855=DIRECTION('center_axis',(0.,-1.,0.));
#7856=DIRECTION('ref_axis',(1.,0.,0.));
#7857=DIRECTION('',(1.,0.,0.));
#7858=DIRECTION('',(1.,0.,0.));
#7859=DIRECTION('',(0.,0.,1.));
#7860=DIRECTION('center_axis',(-1.,0.,0.));
#7861=DIRECTION('ref_axis',(0.,-1.,0.));
#7862=DIRECTION('',(0.,-1.,0.));
#7863=DIRECTION('',(0.,-1.,0.));
#7864=DIRECTION('center_axis',(0.,0.,1.));
#7865=DIRECTION('ref_axis',(1.,0.,0.));
#7866=DIRECTION('center_axis',(0.,0.,1.));
#7867=DIRECTION('ref_axis',(1.,0.,0.));
#7868=DIRECTION('axis',(0.,0.,1.));
#7869=DIRECTION('refdir',(1.,0.,0.));
#7870=DIRECTION('center_axis',(0.,1.,0.));
#7871=DIRECTION('ref_axis',(1.,0.,0.));
#7872=DIRECTION('center_axis',(0.,1.,0.));
#7873=DIRECTION('ref_axis',(1.,0.,0.));
#7874=DIRECTION('',(0.,1.,0.));
#7875=DIRECTION('center_axis',(0.,-1.,0.));
#7876=DIRECTION('ref_axis',(1.,0.,0.));
#7877=DIRECTION('center_axis',(0.,1.,0.));
#7878=DIRECTION('ref_axis',(1.,0.,0.));
#7879=DIRECTION('center_axis',(0.,1.,0.));
#7880=DIRECTION('ref_axis',(1.,0.,0.));
#7881=DIRECTION('center_axis',(0.,1.,0.));
#7882=DIRECTION('ref_axis',(1.,0.,0.));
#7883=DIRECTION('',(0.,1.,0.));
#7884=DIRECTION('center_axis',(0.,-1.,0.));
#7885=DIRECTION('ref_axis',(1.,0.,0.));
#7886=DIRECTION('center_axis',(0.,1.,0.));
#7887=DIRECTION('ref_axis',(1.,0.,0.));
#7888=DIRECTION('center_axis',(0.,1.,0.));
#7889=DIRECTION('ref_axis',(1.,0.,0.));
#7890=DIRECTION('center_axis',(0.,1.,0.));
#7891=DIRECTION('ref_axis',(1.,0.,0.));
#7892=DIRECTION('',(0.,1.,0.));
#7893=DIRECTION('center_axis',(0.,-1.,0.));
#7894=DIRECTION('ref_axis',(1.,0.,0.));
#7895=DIRECTION('center_axis',(0.,1.,0.));
#7896=DIRECTION('ref_axis',(1.,0.,0.));
#7897=DIRECTION('center_axis',(0.,1.,0.));
#7898=DIRECTION('ref_axis',(1.,0.,0.));
#7899=DIRECTION('center_axis',(0.,1.,0.));
#7900=DIRECTION('ref_axis',(1.,0.,0.));
#7901=DIRECTION('',(0.,1.,0.));
#7902=DIRECTION('center_axis',(0.,-1.,0.));
#7903=DIRECTION('ref_axis',(1.,0.,0.));
#7904=DIRECTION('center_axis',(0.,1.,0.));
#7905=DIRECTION('ref_axis',(1.,0.,0.));
#7906=DIRECTION('center_axis',(0.,1.,0.));
#7907=DIRECTION('ref_axis',(1.,0.,0.));
#7908=DIRECTION('center_axis',(0.,1.,0.));
#7909=DIRECTION('ref_axis',(1.,0.,0.));
#7910=DIRECTION('',(0.,1.,0.));
#7911=DIRECTION('center_axis',(0.,1.,0.));
#7912=DIRECTION('ref_axis',(1.,0.,0.));
#7913=DIRECTION('center_axis',(0.,1.,0.));
#7914=DIRECTION('ref_axis',(1.,0.,0.));
#7915=DIRECTION('center_axis',(0.,1.,0.));
#7916=DIRECTION('ref_axis',(1.,0.,0.));
#7917=DIRECTION('center_axis',(0.,1.,0.));
#7918=DIRECTION('ref_axis',(1.,0.,0.));
#7919=DIRECTION('',(0.,1.,0.));
#7920=DIRECTION('center_axis',(0.,1.,0.));
#7921=DIRECTION('ref_axis',(1.,0.,0.));
#7922=DIRECTION('center_axis',(0.,1.,0.));
#7923=DIRECTION('ref_axis',(1.,0.,0.));
#7924=DIRECTION('center_axis',(0.,1.,0.));
#7925=DIRECTION('ref_axis',(1.,0.,0.));
#7926=DIRECTION('center_axis',(0.,1.,0.));
#7927=DIRECTION('ref_axis',(1.,0.,0.));
#7928=DIRECTION('',(0.,1.,0.));
#7929=DIRECTION('center_axis',(0.,1.,0.));
#7930=DIRECTION('ref_axis',(1.,0.,0.));
#7931=DIRECTION('center_axis',(0.,1.,0.));
#7932=DIRECTION('ref_axis',(1.,0.,0.));
#7933=DIRECTION('center_axis',(0.,1.,0.));
#7934=DIRECTION('ref_axis',(1.,0.,0.));
#7935=DIRECTION('center_axis',(0.,1.,0.));
#7936=DIRECTION('ref_axis',(1.,0.,0.));
#7937=DIRECTION('',(0.,1.,0.));
#7938=DIRECTION('center_axis',(0.,1.,0.));
#7939=DIRECTION('ref_axis',(1.,0.,0.));
#7940=DIRECTION('center_axis',(0.,1.,0.));
#7941=DIRECTION('ref_axis',(1.,0.,0.));
#7942=DIRECTION('center_axis',(0.,0.,1.));
#7943=DIRECTION('ref_axis',(1.,0.,0.));
#7944=DIRECTION('',(0.,0.,-1.));
#7945=DIRECTION('center_axis',(0.,0.,-1.));
#7946=DIRECTION('ref_axis',(1.,0.,0.));
#7947=DIRECTION('',(0.,0.,1.));
#7948=DIRECTION('center_axis',(0.,0.,1.));
#7949=DIRECTION('ref_axis',(1.,0.,0.));
#7950=DIRECTION('center_axis',(0.,0.,1.));
#7951=DIRECTION('ref_axis',(-1.,-1.22464679914735E-16,0.));
#7952=DIRECTION('',(0.,0.,1.));
#7953=DIRECTION('center_axis',(0.,0.,1.));
#7954=DIRECTION('ref_axis',(1.,0.,0.));
#7955=DIRECTION('',(0.,0.,-1.));
#7956=DIRECTION('center_axis',(0.,0.,-1.));
#7957=DIRECTION('ref_axis',(1.,0.,0.));
#7958=DIRECTION('center_axis',(0.,0.,1.));
#7959=DIRECTION('ref_axis',(1.,0.,0.));
#7960=DIRECTION('',(-1.,0.,0.));
#7961=DIRECTION('',(1.,0.,0.));
#7962=DIRECTION('center_axis',(0.,0.,1.));
#7963=DIRECTION('ref_axis',(1.,0.,0.));
#7964=DIRECTION('center_axis',(0.,0.,1.));
#7965=DIRECTION('ref_axis',(1.,0.,0.));
#7966=DIRECTION('',(0.,0.,-1.));
#7967=DIRECTION('center_axis',(0.,0.,-1.));
#7968=DIRECTION('ref_axis',(1.,0.,0.));
#7969=DIRECTION('',(0.,0.,1.));
#7970=DIRECTION('center_axis',(0.,0.,1.));
#7971=DIRECTION('ref_axis',(1.,0.,0.));
#7972=DIRECTION('center_axis',(0.,0.,1.));
#7973=DIRECTION('ref_axis',(-1.,-1.22464679914735E-16,0.));
#7974=DIRECTION('',(0.,0.,1.));
#7975=DIRECTION('center_axis',(0.,0.,1.));
#7976=DIRECTION('ref_axis',(1.,0.,0.));
#7977=DIRECTION('',(0.,0.,-1.));
#7978=DIRECTION('center_axis',(0.,0.,-1.));
#7979=DIRECTION('ref_axis',(1.,0.,0.));
#7980=DIRECTION('center_axis',(0.,0.,1.));
#7981=DIRECTION('ref_axis',(1.,0.,0.));
#7982=DIRECTION('',(-1.,0.,0.));
#7983=DIRECTION('',(1.,0.,0.));
#7984=DIRECTION('center_axis',(0.,0.,1.));
#7985=DIRECTION('ref_axis',(1.,0.,0.));
#7986=DIRECTION('center_axis',(0.,0.,1.));
#7987=DIRECTION('ref_axis',(1.,0.,0.));
#7988=DIRECTION('',(0.,0.,-1.));
#7989=DIRECTION('center_axis',(0.,0.,-1.));
#7990=DIRECTION('ref_axis',(1.,0.,0.));
#7991=DIRECTION('',(0.,0.,1.));
#7992=DIRECTION('center_axis',(0.,0.,1.));
#7993=DIRECTION('ref_axis',(1.,0.,0.));
#7994=DIRECTION('center_axis',(0.,0.,1.));
#7995=DIRECTION('ref_axis',(-1.,-1.22464679914735E-16,0.));
#7996=DIRECTION('',(0.,0.,1.));
#7997=DIRECTION('center_axis',(0.,0.,1.));
#7998=DIRECTION('ref_axis',(1.,0.,0.));
#7999=DIRECTION('',(0.,0.,-1.));
#8000=DIRECTION('center_axis',(0.,0.,-1.));
#8001=DIRECTION('ref_axis',(1.,0.,0.));
#8002=DIRECTION('center_axis',(0.,0.,1.));
#8003=DIRECTION('ref_axis',(1.,0.,0.));
#8004=DIRECTION('',(-1.,0.,0.));
#8005=DIRECTION('',(1.,0.,0.));
#8006=DIRECTION('center_axis',(0.,0.,1.));
#8007=DIRECTION('ref_axis',(1.,0.,0.));
#8008=DIRECTION('center_axis',(0.,0.,1.));
#8009=DIRECTION('ref_axis',(1.,0.,0.));
#8010=DIRECTION('',(0.,0.,-1.));
#8011=DIRECTION('center_axis',(0.,0.,-1.));
#8012=DIRECTION('ref_axis',(1.,0.,0.));
#8013=DIRECTION('',(0.,0.,1.));
#8014=DIRECTION('center_axis',(0.,0.,1.));
#8015=DIRECTION('ref_axis',(1.,0.,0.));
#8016=DIRECTION('center_axis',(0.,0.,1.));
#8017=DIRECTION('ref_axis',(-1.,-1.22464679914735E-16,0.));
#8018=DIRECTION('',(0.,0.,1.));
#8019=DIRECTION('center_axis',(0.,0.,1.));
#8020=DIRECTION('ref_axis',(1.,0.,0.));
#8021=DIRECTION('',(0.,0.,-1.));
#8022=DIRECTION('center_axis',(0.,0.,-1.));
#8023=DIRECTION('ref_axis',(1.,0.,0.));
#8024=DIRECTION('center_axis',(0.,0.,1.));
#8025=DIRECTION('ref_axis',(1.,0.,0.));
#8026=DIRECTION('',(-1.,0.,0.));
#8027=DIRECTION('',(1.,0.,0.));
#8028=DIRECTION('center_axis',(0.,0.,1.));
#8029=DIRECTION('ref_axis',(1.,0.,0.));
#8030=DIRECTION('center_axis',(0.,0.,1.));
#8031=DIRECTION('ref_axis',(1.,0.,0.));
#8032=DIRECTION('',(-1.,0.,0.));
#8033=DIRECTION('',(0.,1.,0.));
#8034=DIRECTION('',(1.,0.,0.));
#8035=DIRECTION('center_axis',(0.,0.,1.));
#8036=DIRECTION('ref_axis',(1.,0.,0.));
#8037=DIRECTION('',(1.,0.,0.));
#8038=DIRECTION('',(0.,1.,0.));
#8039=DIRECTION('',(-1.,0.,0.));
#8040=DIRECTION('center_axis',(0.,0.,1.));
#8041=DIRECTION('ref_axis',(1.,0.,0.));
#8042=DIRECTION('',(-1.,0.,0.));
#8043=DIRECTION('',(0.,-1.,0.));
#8044=DIRECTION('',(1.,0.,0.));
#8045=DIRECTION('center_axis',(0.,0.,1.));
#8046=DIRECTION('ref_axis',(1.,0.,0.));
#8047=DIRECTION('',(1.,0.,0.));
#8048=DIRECTION('',(0.,1.,0.));
#8049=DIRECTION('',(-1.,0.,0.));
#8050=DIRECTION('center_axis',(0.,1.,0.));
#8051=DIRECTION('ref_axis',(0.,0.,1.));
#8052=DIRECTION('',(0.,0.,-1.));
#8053=DIRECTION('',(-1.,0.,0.));
#8054=DIRECTION('',(0.,0.,1.));
#8055=DIRECTION('',(1.,0.,0.));
#8056=DIRECTION('',(1.,0.,0.));
#8057=DIRECTION('center_axis',(0.,1.,0.));
#8058=DIRECTION('ref_axis',(1.,0.,0.));
#8059=DIRECTION('center_axis',(0.,0.,1.));
#8060=DIRECTION('ref_axis',(1.,0.,0.));
#8061=DIRECTION('',(-1.,0.,0.));
#8062=DIRECTION('',(0.,-1.,0.));
#8063=DIRECTION('center_axis',(0.,0.,1.));
#8064=DIRECTION('ref_axis',(1.,0.,0.));
#8065=DIRECTION('',(0.,1.,0.));
#8066=DIRECTION('',(-1.,0.,0.));
#8067=DIRECTION('center_axis',(0.,1.,0.));
#8068=DIRECTION('ref_axis',(0.,0.,1.));
#8069=DIRECTION('center_axis',(0.,1.,0.));
#8070=DIRECTION('ref_axis',(1.,0.,0.));
#8071=DIRECTION('',(1.,0.,0.));
#8072=DIRECTION('',(1.,0.,0.));
#8073=DIRECTION('',(0.,0.,-1.));
#8074=DIRECTION('',(-1.,0.,0.));
#8075=DIRECTION('',(0.,0.,1.));
#8076=DIRECTION('center_axis',(0.,0.,1.));
#8077=DIRECTION('ref_axis',(1.,0.,0.));
#8078=DIRECTION('',(-1.,0.,0.));
#8079=DIRECTION('',(0.,1.,0.));
#8080=DIRECTION('center_axis',(0.,0.,1.));
#8081=DIRECTION('ref_axis',(1.,0.,0.));
#8082=DIRECTION('',(0.,1.,0.));
#8083=DIRECTION('',(-1.,0.,0.));
#8084=DIRECTION('center_axis',(0.,0.,1.));
#8085=DIRECTION('ref_axis',(1.,0.,0.));
#8086=DIRECTION('center_axis',(0.,0.,1.));
#8087=DIRECTION('ref_axis',(1.,0.,0.));
#8088=DIRECTION('',(0.,0.,1.));
#8089=DIRECTION('center_axis',(0.,0.,1.));
#8090=DIRECTION('ref_axis',(1.,0.,0.));
#8091=DIRECTION('center_axis',(0.,0.,1.));
#8092=DIRECTION('ref_axis',(1.,0.,0.));
#8093=DIRECTION('',(0.,0.,1.));
#8094=DIRECTION('center_axis',(0.,0.,1.));
#8095=DIRECTION('ref_axis',(1.,0.,0.));
#8096=DIRECTION('center_axis',(0.,0.,1.));
#8097=DIRECTION('ref_axis',(1.,0.,0.));
#8098=DIRECTION('',(0.,0.,1.));
#8099=DIRECTION('center_axis',(0.,0.,1.));
#8100=DIRECTION('ref_axis',(1.,0.,0.));
#8101=DIRECTION('center_axis',(0.,0.,1.));
#8102=DIRECTION('ref_axis',(1.,0.,0.));
#8103=DIRECTION('',(0.,0.,1.));
#8104=DIRECTION('center_axis',(-1.,0.,0.));
#8105=DIRECTION('ref_axis',(0.,0.,1.));
#8106=DIRECTION('',(0.,0.,-1.));
#8107=DIRECTION('',(0.,1.,0.));
#8108=DIRECTION('center_axis',(0.,0.,-1.));
#8109=DIRECTION('ref_axis',(-1.,0.,0.));
#8110=DIRECTION('',(1.,0.,0.));
#8111=DIRECTION('',(0.,1.,0.));
#8112=DIRECTION('center_axis',(1.,0.,0.));
#8113=DIRECTION('ref_axis',(0.,0.,-1.));
#8114=DIRECTION('',(0.,0.,1.));
#8115=DIRECTION('center_axis',(0.,1.,0.));
#8116=DIRECTION('ref_axis',(1.,0.,0.));
#8117=DIRECTION('center_axis',(0.,-1.,0.));
#8118=DIRECTION('ref_axis',(1.,0.,0.));
#8119=DIRECTION('center_axis',(-1.,0.,0.));
#8120=DIRECTION('ref_axis',(0.,0.,1.));
#8121=DIRECTION('',(0.,0.,-1.));
#8122=DIRECTION('',(0.,1.,0.));
#8123=DIRECTION('center_axis',(0.,0.,-1.));
#8124=DIRECTION('ref_axis',(-1.,0.,0.));
#8125=DIRECTION('',(1.,0.,0.));
#8126=DIRECTION('',(0.,1.,0.));
#8127=DIRECTION('center_axis',(1.,0.,0.));
#8128=DIRECTION('ref_axis',(0.,0.,-1.));
#8129=DIRECTION('',(0.,0.,1.));
#8130=DIRECTION('center_axis',(0.,1.,0.));
#8131=DIRECTION('ref_axis',(1.,0.,0.));
#8132=DIRECTION('center_axis',(0.,-1.,0.));
#8133=DIRECTION('ref_axis',(1.,0.,0.));
#8134=DIRECTION('center_axis',(0.,1.,0.));
#8135=DIRECTION('ref_axis',(1.,0.,0.));
#8136=DIRECTION('center_axis',(0.,-1.,0.));
#8137=DIRECTION('ref_axis',(1.,0.,0.));
#8138=DIRECTION('',(0.,-1.,0.));
#8139=DIRECTION('center_axis',(0.,-1.,0.));
#8140=DIRECTION('ref_axis',(1.,0.,0.));
#8141=DIRECTION('center_axis',(0.,1.,0.));
#8142=DIRECTION('ref_axis',(1.,0.,0.));
#8143=DIRECTION('center_axis',(0.,1.,0.));
#8144=DIRECTION('ref_axis',(1.,0.,0.));
#8145=DIRECTION('',(0.,-1.,0.));
#8146=DIRECTION('center_axis',(0.,1.,0.));
#8147=DIRECTION('ref_axis',(1.,0.,0.));
#8148=DIRECTION('center_axis',(0.,1.,0.));
#8149=DIRECTION('ref_axis',(1.,0.,0.));
#8150=DIRECTION('center_axis',(0.,1.,0.));
#8151=DIRECTION('ref_axis',(1.,0.,0.));
#8152=DIRECTION('axis',(0.,0.,1.));
#8153=DIRECTION('refdir',(1.,0.,0.));
#8154=DIRECTION('center_axis',(0.,1.,0.));
#8155=DIRECTION('ref_axis',(1.,0.,0.));
#8156=DIRECTION('center_axis',(0.,-1.,0.));
#8157=DIRECTION('ref_axis',(1.,0.,0.));
#8158=DIRECTION('',(0.,-1.,0.));
#8159=DIRECTION('center_axis',(0.,-1.,0.));
#8160=DIRECTION('ref_axis',(1.,0.,0.));
#8161=DIRECTION('center_axis',(0.,1.,0.));
#8162=DIRECTION('ref_axis',(1.,0.,0.));
#8163=DIRECTION('center_axis',(0.,1.,0.));
#8164=DIRECTION('ref_axis',(1.,0.,0.));
#8165=DIRECTION('',(0.,-1.,0.));
#8166=DIRECTION('center_axis',(0.,1.,0.));
#8167=DIRECTION('ref_axis',(1.,0.,0.));
#8168=DIRECTION('center_axis',(0.,1.,0.));
#8169=DIRECTION('ref_axis',(1.,0.,0.));
#8170=DIRECTION('center_axis',(0.,1.,0.));
#8171=DIRECTION('ref_axis',(1.,0.,0.));
#8172=DIRECTION('axis',(0.,0.,1.));
#8173=DIRECTION('refdir',(1.,0.,0.));
#8174=DIRECTION('center_axis',(0.,1.,0.));
#8175=DIRECTION('ref_axis',(1.,0.,0.));
#8176=DIRECTION('center_axis',(0.,1.,0.));
#8177=DIRECTION('ref_axis',(1.,0.,0.));
#8178=DIRECTION('',(0.,1.,0.));
#8179=DIRECTION('center_axis',(0.,-1.,0.));
#8180=DIRECTION('ref_axis',(1.,0.,0.));
#8181=DIRECTION('center_axis',(0.,1.,0.));
#8182=DIRECTION('ref_axis',(1.,0.,0.));
#8183=DIRECTION('center_axis',(0.,1.,0.));
#8184=DIRECTION('ref_axis',(1.,0.,0.));
#8185=DIRECTION('',(0.,1.,0.));
#8186=DIRECTION('center_axis',(0.,-1.,0.));
#8187=DIRECTION('ref_axis',(1.,0.,0.));
#8188=DIRECTION('center_axis',(0.,1.,0.));
#8189=DIRECTION('ref_axis',(1.,0.,0.));
#8190=DIRECTION('center_axis',(0.,1.,0.));
#8191=DIRECTION('ref_axis',(1.,0.,0.));
#8192=DIRECTION('',(0.,1.,0.));
#8193=DIRECTION('center_axis',(0.,-1.,0.));
#8194=DIRECTION('ref_axis',(1.,0.,0.));
#8195=DIRECTION('center_axis',(0.,1.,0.));
#8196=DIRECTION('ref_axis',(1.,0.,0.));
#8197=DIRECTION('center_axis',(0.,1.,0.));
#8198=DIRECTION('ref_axis',(1.,0.,0.));
#8199=DIRECTION('',(0.,1.,0.));
#8200=DIRECTION('center_axis',(0.,-1.,0.));
#8201=DIRECTION('ref_axis',(1.,0.,0.));
#8202=DIRECTION('center_axis',(0.,1.,0.));
#8203=DIRECTION('ref_axis',(1.,0.,0.));
#8204=DIRECTION('center_axis',(0.,1.,0.));
#8205=DIRECTION('ref_axis',(1.,0.,0.));
#8206=DIRECTION('',(0.,-1.,0.));
#8207=DIRECTION('center_axis',(0.,-1.,0.));
#8208=DIRECTION('ref_axis',(1.,0.,0.));
#8209=DIRECTION('center_axis',(0.,1.,0.));
#8210=DIRECTION('ref_axis',(1.,0.,0.));
#8211=DIRECTION('center_axis',(0.,-1.,0.));
#8212=DIRECTION('ref_axis',(1.,0.,0.));
#8213=DIRECTION('center_axis',(0.,1.,0.));
#8214=DIRECTION('ref_axis',(1.,0.,0.));
#8215=DIRECTION('',(0.,-1.,0.));
#8216=DIRECTION('center_axis',(0.,-1.,0.));
#8217=DIRECTION('ref_axis',(1.,0.,0.));
#8218=DIRECTION('center_axis',(0.,1.,0.));
#8219=DIRECTION('ref_axis',(1.,0.,0.));
#8220=DIRECTION('center_axis',(0.,1.,0.));
#8221=DIRECTION('ref_axis',(1.,0.,0.));
#8222=DIRECTION('',(0.,-1.,0.));
#8223=DIRECTION('center_axis',(0.,1.,0.));
#8224=DIRECTION('ref_axis',(1.,0.,0.));
#8225=DIRECTION('center_axis',(0.,1.,0.));
#8226=DIRECTION('ref_axis',(1.,0.,0.));
#8227=DIRECTION('center_axis',(0.,1.,0.));
#8228=DIRECTION('ref_axis',(1.,0.,0.));
#8229=DIRECTION('axis',(0.,0.,1.));
#8230=DIRECTION('refdir',(1.,0.,0.));
#8231=DIRECTION('center_axis',(0.,1.,0.));
#8232=DIRECTION('ref_axis',(1.,0.,0.));
#8233=DIRECTION('center_axis',(0.,1.,0.));
#8234=DIRECTION('ref_axis',(1.,0.,0.));
#8235=DIRECTION('',(0.,1.,0.));
#8236=DIRECTION('center_axis',(0.,-1.,0.));
#8237=DIRECTION('ref_axis',(1.,0.,0.));
#8238=DIRECTION('center_axis',(0.,1.,0.));
#8239=DIRECTION('ref_axis',(1.,0.,0.));
#8240=DIRECTION('center_axis',(0.,1.,0.));
#8241=DIRECTION('ref_axis',(1.,0.,0.));
#8242=DIRECTION('',(0.,1.,0.));
#8243=DIRECTION('center_axis',(0.,-1.,0.));
#8244=DIRECTION('ref_axis',(1.,0.,0.));
#8245=DIRECTION('center_axis',(0.,1.,0.));
#8246=DIRECTION('ref_axis',(1.,0.,0.));
#8247=DIRECTION('center_axis',(0.,1.,0.));
#8248=DIRECTION('ref_axis',(1.,0.,0.));
#8249=DIRECTION('',(0.,1.,0.));
#8250=DIRECTION('center_axis',(0.,-1.,0.));
#8251=DIRECTION('ref_axis',(1.,0.,0.));
#8252=DIRECTION('center_axis',(0.,1.,0.));
#8253=DIRECTION('ref_axis',(1.,0.,0.));
#8254=DIRECTION('center_axis',(0.,1.,0.));
#8255=DIRECTION('ref_axis',(1.,0.,0.));
#8256=DIRECTION('',(0.,1.,0.));
#8257=DIRECTION('center_axis',(0.,-1.,0.));
#8258=DIRECTION('ref_axis',(1.,0.,0.));
#8259=DIRECTION('center_axis',(0.,1.,0.));
#8260=DIRECTION('ref_axis',(1.,0.,0.));
#8261=DIRECTION('center_axis',(0.,1.,0.));
#8262=DIRECTION('ref_axis',(1.,0.,0.));
#8263=DIRECTION('',(0.,-1.,0.));
#8264=DIRECTION('center_axis',(0.,1.,0.));
#8265=DIRECTION('ref_axis',(1.,0.,0.));
#8266=DIRECTION('center_axis',(0.,1.,0.));
#8267=DIRECTION('ref_axis',(1.,0.,0.));
#8268=DIRECTION('center_axis',(0.,-1.,0.));
#8269=DIRECTION('ref_axis',(1.,0.,0.));
#8270=DIRECTION('center_axis',(0.,1.,0.));
#8271=DIRECTION('ref_axis',(1.,0.,0.));
#8272=DIRECTION('center_axis',(0.,-1.,0.));
#8273=DIRECTION('ref_axis',(1.,0.,0.));
#8274=DIRECTION('',(0.,-1.,0.));
#8275=DIRECTION('center_axis',(0.,1.,0.));
#8276=DIRECTION('ref_axis',(1.,0.,0.));
#8277=DIRECTION('center_axis',(0.,1.,0.));
#8278=DIRECTION('ref_axis',(1.,0.,0.));
#8279=DIRECTION('',(0.,-1.,0.));
#8280=DIRECTION('center_axis',(0.,1.,0.));
#8281=DIRECTION('ref_axis',(1.,0.,0.));
#8282=DIRECTION('center_axis',(0.,1.,0.));
#8283=DIRECTION('ref_axis',(1.,0.,0.));
#8284=DIRECTION('center_axis',(0.,1.,0.));
#8285=DIRECTION('ref_axis',(1.,0.,0.));
#8286=DIRECTION('axis',(0.,0.,1.));
#8287=DIRECTION('refdir',(1.,0.,0.));
#8288=DIRECTION('center_axis',(0.,1.,0.));
#8289=DIRECTION('ref_axis',(-1.,0.,0.));
#8290=DIRECTION('',(-1.,0.,0.));
#8291=DIRECTION('',(0.,0.,1.));
#8292=DIRECTION('',(-1.,0.,0.));
#8293=DIRECTION('',(0.,0.,1.));
#8294=DIRECTION('center_axis',(1.,0.,0.));
#8295=DIRECTION('ref_axis',(0.,1.,0.));
#8296=DIRECTION('',(0.,1.,0.));
#8297=DIRECTION('',(0.,1.,0.));
#8298=DIRECTION('',(0.,0.,1.));
#8299=DIRECTION('center_axis',(0.,-1.,0.));
#8300=DIRECTION('ref_axis',(1.,0.,0.));
#8301=DIRECTION('',(1.,0.,0.));
#8302=DIRECTION('',(1.,0.,0.));
#8303=DIRECTION('',(0.,0.,1.));
#8304=DIRECTION('center_axis',(-1.,0.,0.));
#8305=DIRECTION('ref_axis',(0.,-1.,0.));
#8306=DIRECTION('',(0.,-1.,0.));
#8307=DIRECTION('',(0.,-1.,0.));
#8308=DIRECTION('center_axis',(0.,0.,1.));
#8309=DIRECTION('ref_axis',(1.,0.,0.));
#8310=DIRECTION('center_axis',(0.,0.,1.));
#8311=DIRECTION('ref_axis',(1.,0.,0.));
#8312=DIRECTION('axis',(0.,0.,1.));
#8313=DIRECTION('refdir',(1.,0.,0.));
#8314=DIRECTION('center_axis',(0.,1.,0.));
#8315=DIRECTION('ref_axis',(-1.,0.,0.));
#8316=DIRECTION('',(-1.,0.,0.));
#8317=DIRECTION('',(0.,0.,1.));
#8318=DIRECTION('',(-1.,0.,0.));
#8319=DIRECTION('',(0.,0.,1.));
#8320=DIRECTION('center_axis',(1.,0.,0.));
#8321=DIRECTION('ref_axis',(0.,1.,0.));
#8322=DIRECTION('',(0.,1.,0.));
#8323=DIRECTION('',(0.,1.,0.));
#8324=DIRECTION('',(0.,0.,1.));
#8325=DIRECTION('center_axis',(0.,-1.,0.));
#8326=DIRECTION('ref_axis',(1.,0.,0.));
#8327=DIRECTION('',(1.,0.,0.));
#8328=DIRECTION('',(1.,0.,0.));
#8329=DIRECTION('',(0.,0.,1.));
#8330=DIRECTION('center_axis',(-1.,0.,0.));
#8331=DIRECTION('ref_axis',(0.,-1.,0.));
#8332=DIRECTION('',(0.,-1.,0.));
#8333=DIRECTION('',(0.,-1.,0.));
#8334=DIRECTION('center_axis',(0.,0.,1.));
#8335=DIRECTION('ref_axis',(1.,0.,0.));
#8336=DIRECTION('center_axis',(0.,0.,1.));
#8337=DIRECTION('ref_axis',(1.,0.,0.));
#8338=DIRECTION('axis',(0.,0.,1.));
#8339=DIRECTION('refdir',(1.,0.,0.));
#8340=DIRECTION('axis',(0.,0.,1.));
#8341=DIRECTION('refdir',(1.,0.,0.));
#8342=DIRECTION('center_axis',(0.,-1.,0.));
#8343=DIRECTION('ref_axis',(0.,0.,-1.));
#8344=DIRECTION('center_axis',(0.,-1.,0.));
#8345=DIRECTION('ref_axis',(1.,0.,0.));
#8346=DIRECTION('center_axis',(0.,-1.,0.));
#8347=DIRECTION('ref_axis',(1.,0.,0.));
#8348=DIRECTION('center_axis',(1.,0.,1.22464679914735E-16));
#8349=DIRECTION('ref_axis',(-1.22464679914735E-16,0.,1.));
#8350=DIRECTION('center_axis',(0.,1.,0.));
#8351=DIRECTION('ref_axis',(1.,0.,0.));
#8352=DIRECTION('center_axis',(0.,1.,0.));
#8353=DIRECTION('ref_axis',(1.,0.,0.));
#8354=DIRECTION('center_axis',(0.,-1.,0.));
#8355=DIRECTION('ref_axis',(1.,0.,0.));
#8356=DIRECTION('',(0.,1.,0.));
#8357=DIRECTION('center_axis',(0.,-1.,0.));
#8358=DIRECTION('ref_axis',(1.,0.,0.));
#8359=DIRECTION('center_axis',(0.,-1.,0.));
#8360=DIRECTION('ref_axis',(1.,0.,0.));
#8361=DIRECTION('center_axis',(0.,-1.,0.));
#8362=DIRECTION('ref_axis',(1.,0.,0.));
#8363=DIRECTION('',(0.,1.,0.));
#8364=DIRECTION('center_axis',(0.,-1.,0.));
#8365=DIRECTION('ref_axis',(1.,0.,0.));
#8366=DIRECTION('center_axis',(0.,1.,0.));
#8367=DIRECTION('ref_axis',(1.,0.,0.));
#8368=DIRECTION('',(-0.707106781186548,0.707106781186547,-8.65956056235494E-17));
#8369=DIRECTION('center_axis',(0.,-1.,0.));
#8370=DIRECTION('ref_axis',(1.,0.,0.));
#8371=DIRECTION('center_axis',(0.,1.,0.));
#8372=DIRECTION('ref_axis',(0.,0.,1.));
#8373=DIRECTION('center_axis',(0.,-1.,0.));
#8374=DIRECTION('ref_axis',(1.,0.,0.));
#8375=DIRECTION('center_axis',(0.,-1.,0.));
#8376=DIRECTION('ref_axis',(1.,0.,0.));
#8377=DIRECTION('',(0.,1.,0.));
#8378=DIRECTION('center_axis',(0.,-1.,0.));
#8379=DIRECTION('ref_axis',(0.,0.,-1.));
#8380=DIRECTION('center_axis',(0.,-1.,0.));
#8381=DIRECTION('ref_axis',(1.,0.,0.));
#8382=DIRECTION('center_axis',(0.,-1.,0.));
#8383=DIRECTION('ref_axis',(1.,0.,0.));
#8384=DIRECTION('',(0.707106781186548,0.707106781186547,8.65956056235494E-17));
#8385=DIRECTION('axis',(0.,0.,1.));
#8386=DIRECTION('refdir',(1.,0.,0.));
#8387=DIRECTION('center_axis',(0.,-1.,0.));
#8388=DIRECTION('ref_axis',(0.,0.,-1.));
#8389=DIRECTION('center_axis',(0.,-1.,0.));
#8390=DIRECTION('ref_axis',(1.,0.,0.));
#8391=DIRECTION('center_axis',(0.,-1.,0.));
#8392=DIRECTION('ref_axis',(1.,0.,0.));
#8393=DIRECTION('center_axis',(1.,0.,1.22464679914735E-16));
#8394=DIRECTION('ref_axis',(-1.22464679914735E-16,0.,1.));
#8395=DIRECTION('center_axis',(0.,1.,0.));
#8396=DIRECTION('ref_axis',(1.,0.,0.));
#8397=DIRECTION('center_axis',(0.,1.,0.));
#8398=DIRECTION('ref_axis',(1.,0.,0.));
#8399=DIRECTION('center_axis',(0.,-1.,0.));
#8400=DIRECTION('ref_axis',(1.,0.,0.));
#8401=DIRECTION('center_axis',(0.,-1.,0.));
#8402=DIRECTION('ref_axis',(1.,0.,0.));
#8403=DIRECTION('',(0.,1.,0.));
#8404=DIRECTION('center_axis',(0.,1.,0.));
#8405=DIRECTION('ref_axis',(0.,0.,1.));
#8406=DIRECTION('center_axis',(0.,-1.,0.));
#8407=DIRECTION('ref_axis',(1.,0.,0.));
#8408=DIRECTION('center_axis',(0.,-1.,0.));
#8409=DIRECTION('ref_axis',(1.,0.,0.));
#8410=DIRECTION('center_axis',(0.,-1.,0.));
#8411=DIRECTION('ref_axis',(1.,0.,0.));
#8412=DIRECTION('center_axis',(0.,-1.,0.));
#8413=DIRECTION('ref_axis',(1.,0.,0.));
#8414=DIRECTION('',(0.707106781186548,0.707106781186547,8.65956056235494E-17));
#8415=DIRECTION('center_axis',(0.,-1.,0.));
#8416=DIRECTION('ref_axis',(1.,0.,0.));
#8417=DIRECTION('center_axis',(0.,-1.,0.));
#8418=DIRECTION('ref_axis',(1.,0.,0.));
#8419=DIRECTION('',(0.,1.,0.));
#8420=DIRECTION('center_axis',(0.,1.,0.));
#8421=DIRECTION('ref_axis',(1.,0.,0.));
#8422=DIRECTION('center_axis',(0.,-1.,0.));
#8423=DIRECTION('ref_axis',(1.,0.,0.));
#8424=DIRECTION('',(-0.707106781186548,0.707106781186547,-8.65956056235494E-17));
#8425=DIRECTION('center_axis',(0.,-1.,0.));
#8426=DIRECTION('ref_axis',(0.,0.,-1.));
#8427=DIRECTION('center_axis',(0.,-1.,0.));
#8428=DIRECTION('ref_axis',(1.,0.,0.));
#8429=DIRECTION('',(0.,1.,0.));
#8430=DIRECTION('axis',(0.,0.,1.));
#8431=DIRECTION('refdir',(1.,0.,0.));
#8432=DIRECTION('center_axis',(0.,0.,1.));
#8433=DIRECTION('ref_axis',(1.,0.,0.));
#8434=DIRECTION('center_axis',(1.22464679914735E-16,-1.,0.));
#8435=DIRECTION('ref_axis',(-1.,-1.22464679914735E-16,0.));
#8436=DIRECTION('center_axis',(0.642787609686539,0.,0.766044443118978));
#8437=DIRECTION('ref_axis',(0.766044443118978,0.,-0.642787609686539));
#8438=DIRECTION('center_axis',(9.38133875270273E-17,-1.,-7.87187788734199E-17));
#8439=DIRECTION('ref_axis',(-0.766044443118978,-1.22464679914735E-16,0.642787609686539));
#8440=DIRECTION('center_axis',(0.984807753012208,0.,0.173648177666931));
#8441=DIRECTION('ref_axis',(0.17364817766693,0.,-0.984807753012208));
#8442=DIRECTION('center_axis',(2.12657684957577E-17,-1.,-1.2060416625019E-16));
#8443=DIRECTION('ref_axis',(-0.17364817766693,-1.22464679914735E-16,0.984807753012208));
#8444=DIRECTION('center_axis',(0.866025403784439,0.,-0.5));
#8445=DIRECTION('ref_axis',(-0.5,0.,-0.866025403784439));
#8446=DIRECTION('center_axis',(-6.12323399573676E-17,-1.,-1.06057523872491E-16));
#8447=DIRECTION('ref_axis',(0.5,-1.22464679914735E-16,0.866025403784439));
#8448=DIRECTION('center_axis',(0.342020143325669,0.,-0.939692620785908));
#8449=DIRECTION('ref_axis',(-0.939692620785908,0.,-0.342020143325669));
#8450=DIRECTION('center_axis',(-1.15079156022785E-16,-1.,-4.18853873767699E-17));
#8451=DIRECTION('ref_axis',(0.939692620785908,-1.22464679914735E-16,0.342020143325669));
#8452=DIRECTION('center_axis',(-0.342020143325669,0.,-0.939692620785908));
#8453=DIRECTION('ref_axis',(-0.939692620785909,0.,0.342020143325669));
#8454=DIRECTION('center_axis',(-1.15079156022785E-16,-1.,4.18853873767699E-17));
#8455=DIRECTION('ref_axis',(0.939692620785908,-1.22464679914735E-16,-0.342020143325669));
#8456=DIRECTION('center_axis',(-0.866025403784438,0.,-0.5));
#8457=DIRECTION('ref_axis',(-0.5,0.,0.866025403784438));
#8458=DIRECTION('center_axis',(-6.12323399573677E-17,-1.,1.06057523872491E-16));
#8459=DIRECTION('ref_axis',(0.5,-1.22464679914735E-16,-0.866025403784438));
#8460=DIRECTION('center_axis',(-0.984807753012208,0.,0.17364817766693));
#8461=DIRECTION('ref_axis',(0.17364817766693,0.,0.984807753012208));
#8462=DIRECTION('center_axis',(2.12657684957577E-17,-1.,1.2060416625019E-16));
#8463=DIRECTION('ref_axis',(-0.17364817766693,-1.22464679914735E-16,-0.984807753012208));
#8464=DIRECTION('center_axis',(-0.64278760968654,0.,0.766044443118978));
#8465=DIRECTION('ref_axis',(0.766044443118978,0.,0.64278760968654));
#8466=DIRECTION('center_axis',(9.38133875270273E-17,-1.,7.87187788734199E-17));
#8467=DIRECTION('ref_axis',(-0.766044443118978,-1.22464679914735E-16,-0.64278760968654));
#8468=DIRECTION('axis',(0.,0.,1.));
#8469=DIRECTION('refdir',(1.,0.,0.));
#8470=DIRECTION('center_axis',(0.,0.,1.));
#8471=DIRECTION('ref_axis',(1.,0.,0.));
#8472=DIRECTION('center_axis',(0.,-1.,0.));
#8473=DIRECTION('ref_axis',(0.,0.,-1.));
#8474=DIRECTION('center_axis',(0.,-1.,0.));
#8475=DIRECTION('ref_axis',(0.,0.,-1.));
#8476=DIRECTION('center_axis',(0.,1.,0.));
#8477=DIRECTION('ref_axis',(1.,0.,0.));
#8478=DIRECTION('center_axis',(0.,1.,0.));
#8479=DIRECTION('ref_axis',(1.,0.,0.));
#8480=DIRECTION('center_axis',(0.,1.,0.));
#8481=DIRECTION('ref_axis',(1.,0.,0.));
#8482=DIRECTION('center_axis',(0.,1.,0.));
#8483=DIRECTION('ref_axis',(1.,0.,0.));
#8484=DIRECTION('center_axis',(0.,1.,0.));
#8485=DIRECTION('ref_axis',(1.,0.,0.));
#8486=DIRECTION('',(0.,-1.,0.));
#8487=DIRECTION('center_axis',(0.,-1.,0.));
#8488=DIRECTION('ref_axis',(1.,0.,0.));
#8489=DIRECTION('center_axis',(0.,1.,0.));
#8490=DIRECTION('ref_axis',(1.,0.,0.));
#8491=DIRECTION('center_axis',(0.,1.,0.));
#8492=DIRECTION('ref_axis',(1.,0.,0.));
#8493=DIRECTION('center_axis',(0.,1.,0.));
#8494=DIRECTION('ref_axis',(1.,0.,0.));
#8495=DIRECTION('center_axis',(0.,1.,0.));
#8496=DIRECTION('ref_axis',(1.,0.,0.));
#8497=DIRECTION('center_axis',(0.,1.,0.));
#8498=DIRECTION('ref_axis',(1.,0.,0.));
#8499=DIRECTION('center_axis',(0.,1.,0.));
#8500=DIRECTION('ref_axis',(1.,0.,0.));
#8501=DIRECTION('center_axis',(0.,1.,0.));
#8502=DIRECTION('ref_axis',(1.,0.,0.));
#8503=DIRECTION('center_axis',(0.,-1.,0.));
#8504=DIRECTION('ref_axis',(1.,0.,0.));
#8505=DIRECTION('center_axis',(0.,-1.,0.));
#8506=DIRECTION('ref_axis',(0.,0.,-1.));
#8507=DIRECTION('center_axis',(0.,0.,1.));
#8508=DIRECTION('ref_axis',(1.,0.,0.));
#8509=DIRECTION('center_axis',(0.,-1.,0.));
#8510=DIRECTION('ref_axis',(0.,0.,-1.));
#8511=DIRECTION('center_axis',(0.,1.,0.));
#8512=DIRECTION('ref_axis',(1.,0.,0.));
#8513=DIRECTION('center_axis',(0.,-1.,0.));
#8514=DIRECTION('ref_axis',(1.,0.,0.));
#8515=DIRECTION('center_axis',(0.,-1.,0.));
#8516=DIRECTION('ref_axis',(0.,0.,-1.));
#8517=DIRECTION('center_axis',(0.,0.,1.));
#8518=DIRECTION('ref_axis',(1.,0.,0.));
#8519=DIRECTION('center_axis',(0.,-1.,0.));
#8520=DIRECTION('ref_axis',(0.,0.,-1.));
#8521=DIRECTION('center_axis',(0.,1.,0.));
#8522=DIRECTION('ref_axis',(1.,0.,0.));
#8523=DIRECTION('center_axis',(0.,-1.,0.));
#8524=DIRECTION('ref_axis',(1.,0.,0.));
#8525=DIRECTION('center_axis',(0.,-1.,0.));
#8526=DIRECTION('ref_axis',(0.,0.,-1.));
#8527=DIRECTION('center_axis',(0.,0.,1.));
#8528=DIRECTION('ref_axis',(1.,0.,0.));
#8529=DIRECTION('center_axis',(0.,-1.,0.));
#8530=DIRECTION('ref_axis',(0.,0.,-1.));
#8531=DIRECTION('center_axis',(0.,1.,0.));
#8532=DIRECTION('ref_axis',(1.,0.,0.));
#8533=DIRECTION('center_axis',(0.,-1.,0.));
#8534=DIRECTION('ref_axis',(1.,0.,0.));
#8535=DIRECTION('center_axis',(0.,-1.,0.));
#8536=DIRECTION('ref_axis',(1.,0.,0.));
#8537=DIRECTION('center_axis',(0.,-1.,0.));
#8538=DIRECTION('ref_axis',(0.,0.,-1.));
#8539=DIRECTION('center_axis',(0.,0.,1.));
#8540=DIRECTION('ref_axis',(1.,0.,0.));
#8541=DIRECTION('center_axis',(0.,-1.,0.));
#8542=DIRECTION('ref_axis',(0.,0.,-1.));
#8543=DIRECTION('center_axis',(0.,1.,0.));
#8544=DIRECTION('ref_axis',(1.,0.,0.));
#8545=DIRECTION('center_axis',(0.,-1.,0.));
#8546=DIRECTION('ref_axis',(1.,0.,0.));
#8547=DIRECTION('center_axis',(0.,-1.,0.));
#8548=DIRECTION('ref_axis',(0.,0.,-1.));
#8549=DIRECTION('center_axis',(0.,0.,1.));
#8550=DIRECTION('ref_axis',(1.,0.,0.));
#8551=DIRECTION('center_axis',(0.,-1.,0.));
#8552=DIRECTION('ref_axis',(0.,0.,-1.));
#8553=DIRECTION('center_axis',(0.,1.,0.));
#8554=DIRECTION('ref_axis',(1.,0.,0.));
#8555=DIRECTION('center_axis',(0.,-1.,0.));
#8556=DIRECTION('ref_axis',(1.,0.,0.));
#8557=DIRECTION('center_axis',(0.,-1.,0.));
#8558=DIRECTION('ref_axis',(0.,0.,-1.));
#8559=DIRECTION('center_axis',(0.,0.,1.));
#8560=DIRECTION('ref_axis',(1.,0.,0.));
#8561=DIRECTION('center_axis',(0.,-1.,0.));
#8562=DIRECTION('ref_axis',(0.,0.,-1.));
#8563=DIRECTION('center_axis',(0.,1.,0.));
#8564=DIRECTION('ref_axis',(1.,0.,0.));
#8565=DIRECTION('center_axis',(0.,-1.,0.));
#8566=DIRECTION('ref_axis',(1.,0.,0.));
#8567=DIRECTION('center_axis',(0.,-1.,0.));
#8568=DIRECTION('ref_axis',(0.,0.,-1.));
#8569=DIRECTION('center_axis',(0.,0.,1.));
#8570=DIRECTION('ref_axis',(1.,0.,0.));
#8571=DIRECTION('center_axis',(0.,-1.,0.));
#8572=DIRECTION('ref_axis',(0.,0.,-1.));
#8573=DIRECTION('center_axis',(0.,1.,0.));
#8574=DIRECTION('ref_axis',(1.,0.,0.));
#8575=DIRECTION('center_axis',(0.,1.,0.));
#8576=DIRECTION('ref_axis',(1.,0.,0.));
#8577=DIRECTION('',(0.,1.,0.));
#8578=DIRECTION('center_axis',(0.,-1.,0.));
#8579=DIRECTION('ref_axis',(1.,0.,0.));
#8580=DIRECTION('center_axis',(0.,-1.,0.));
#8581=DIRECTION('ref_axis',(1.,0.,0.));
#8582=DIRECTION('center_axis',(0.,1.,0.));
#8583=DIRECTION('ref_axis',(1.,0.,0.));
#8584=DIRECTION('center_axis',(0.,-1.,0.));
#8585=DIRECTION('ref_axis',(0.,0.,-1.));
#8586=DIRECTION('center_axis',(0.,0.,1.));
#8587=DIRECTION('ref_axis',(1.,0.,0.));
#8588=DIRECTION('center_axis',(0.,-1.,0.));
#8589=DIRECTION('ref_axis',(0.,0.,-1.));
#8590=DIRECTION('center_axis',(0.,-1.,0.));
#8591=DIRECTION('ref_axis',(-1.,0.,0.));
#8592=DIRECTION('center_axis',(0.,1.,0.));
#8593=DIRECTION('ref_axis',(1.,0.,0.));
#8594=DIRECTION('axis',(0.,0.,1.));
#8595=DIRECTION('refdir',(1.,0.,0.));
#8596=DIRECTION('center_axis',(0.,1.,0.));
#8597=DIRECTION('ref_axis',(0.,0.,1.));
#8598=DIRECTION('center_axis',(0.,-1.,0.));
#8599=DIRECTION('ref_axis',(1.,0.,0.));
#8600=DIRECTION('center_axis',(0.,-1.,0.));
#8601=DIRECTION('ref_axis',(1.,0.,0.));
#8602=DIRECTION('center_axis',(0.,-1.,0.));
#8603=DIRECTION('ref_axis',(1.,0.,0.));
#8604=DIRECTION('center_axis',(0.,-1.,0.));
#8605=DIRECTION('ref_axis',(1.,0.,0.));
#8606=DIRECTION('',(0.,1.,0.));
#8607=DIRECTION('center_axis',(0.,-1.,0.));
#8608=DIRECTION('ref_axis',(0.,0.,-1.));
#8609=DIRECTION('center_axis',(0.,-1.,0.));
#8610=DIRECTION('ref_axis',(1.,0.,0.));
#8611=DIRECTION('center_axis',(0.,-1.,0.));
#8612=DIRECTION('ref_axis',(1.,0.,0.));
#8613=DIRECTION('',(0.,1.,0.));
#8614=DIRECTION('center_axis',(0.,1.,0.));
#8615=DIRECTION('ref_axis',(0.,0.,1.));
#8616=DIRECTION('center_axis',(0.,-1.,0.));
#8617=DIRECTION('ref_axis',(1.,0.,0.));
#8618=DIRECTION('center_axis',(0.,-1.,0.));
#8619=DIRECTION('ref_axis',(1.,0.,0.));
#8620=DIRECTION('center_axis',(0.,-1.,0.));
#8621=DIRECTION('ref_axis',(1.,0.,0.));
#8622=DIRECTION('center_axis',(0.,-1.,0.));
#8623=DIRECTION('ref_axis',(1.,0.,0.));
#8624=DIRECTION('',(0.,1.,0.));
#8625=DIRECTION('center_axis',(0.,-1.,0.));
#8626=DIRECTION('ref_axis',(0.,0.,-1.));
#8627=DIRECTION('center_axis',(0.,-1.,0.));
#8628=DIRECTION('ref_axis',(1.,0.,0.));
#8629=DIRECTION('center_axis',(0.,-1.,0.));
#8630=DIRECTION('ref_axis',(1.,0.,0.));
#8631=DIRECTION('',(0.,1.,0.));
#8632=DIRECTION('',(0.,0.,1.));
#8633=DIRECTION('',(1.,0.,0.));
#8634=DIRECTION('',(0.,0.,1.));
#8635=DIRECTION('',(1.,0.,0.));
#8636=DIRECTION('',(0.,0.,1.));
#8637=DIRECTION('',(1.,0.,0.));
#8638=DIRECTION('',(0.,0.,1.));
#8639=DIRECTION('',(1.,0.,0.));
#8640=DIRECTION('',(0.,0.,1.));
#8641=DIRECTION('',(1.,0.,0.));
#8642=DIRECTION('axis',(0.,0.,1.));
#8643=DIRECTION('refdir',(1.,0.,0.));
#8644=DIRECTION('center_axis',(0.,1.,0.));
#8645=DIRECTION('ref_axis',(0.,0.,1.));
#8646=DIRECTION('center_axis',(0.,-1.,0.));
#8647=DIRECTION('ref_axis',(1.,0.,0.));
#8648=DIRECTION('center_axis',(0.,-1.,0.));
#8649=DIRECTION('ref_axis',(1.,0.,0.));
#8650=DIRECTION('center_axis',(0.,-1.,0.));
#8651=DIRECTION('ref_axis',(1.,0.,0.));
#8652=DIRECTION('',(0.707106781186548,0.707106781186547,8.65956056235494E-17));
#8653=DIRECTION('center_axis',(0.,-1.,0.));
#8654=DIRECTION('ref_axis',(1.,0.,0.));
#8655=DIRECTION('center_axis',(0.,-1.,0.));
#8656=DIRECTION('ref_axis',(1.,0.,0.));
#8657=DIRECTION('',(0.,1.,0.));
#8658=DIRECTION('center_axis',(0.,1.,0.));
#8659=DIRECTION('ref_axis',(1.,0.,0.));
#8660=DIRECTION('center_axis',(0.,-1.,0.));
#8661=DIRECTION('ref_axis',(1.,0.,0.));
#8662=DIRECTION('',(-0.707106781186547,0.707106781186548,-8.65956056235493E-17));
#8663=DIRECTION('center_axis',(0.,-1.,0.));
#8664=DIRECTION('ref_axis',(0.,0.,-1.));
#8665=DIRECTION('center_axis',(0.,-1.,0.));
#8666=DIRECTION('ref_axis',(1.,0.,0.));
#8667=DIRECTION('center_axis',(0.,1.,0.));
#8668=DIRECTION('ref_axis',(1.,0.,0.));
#8669=DIRECTION('center_axis',(0.,1.,0.));
#8670=DIRECTION('ref_axis',(1.,0.,0.));
#8671=DIRECTION('',(-0.447213595499958,0.894427190999916,-5.47678698264203E-17));
#8672=DIRECTION('center_axis',(0.,-1.,0.));
#8673=DIRECTION('ref_axis',(1.,0.,0.));
#8674=DIRECTION('center_axis',(0.,1.,0.));
#8675=DIRECTION('ref_axis',(1.,0.,0.));
#8676=DIRECTION('',(0.,1.,0.));
#8677=DIRECTION('center_axis',(0.,1.,0.));
#8678=DIRECTION('ref_axis',(1.,0.,0.));
#8679=DIRECTION('center_axis',(0.,-1.,0.));
#8680=DIRECTION('ref_axis',(1.,0.,0.));
#8681=DIRECTION('',(-0.707106781186547,0.707106781186548,-8.65956056235493E-17));
#8682=DIRECTION('center_axis',(0.,-1.,0.));
#8683=DIRECTION('ref_axis',(0.,0.,-1.));
#8684=DIRECTION('center_axis',(0.866025403784439,0.,-0.5));
#8685=DIRECTION('ref_axis',(0.5,0.,0.866025403784439));
#8686=DIRECTION('',(-0.5,0.,-0.866025403784439));
#8687=DIRECTION('',(0.,-1.,0.));
#8688=DIRECTION('',(0.5,0.,0.866025403784439));
#8689=DIRECTION('',(0.,-1.,0.));
#8690=DIRECTION('center_axis',(1.92296268638356E-16,0.,-1.));
#8691=DIRECTION('ref_axis',(1.,0.,1.92296268638356E-16));
#8692=DIRECTION('',(-1.,0.,-1.92296268638356E-16));
#8693=DIRECTION('',(0.,-1.,0.));
#8694=DIRECTION('',(1.,0.,1.92296268638356E-16));
#8695=DIRECTION('center_axis',(-0.866025403784439,0.,-0.5));
#8696=DIRECTION('ref_axis',(0.5,0.,-0.866025403784439));
#8697=DIRECTION('',(-0.5,0.,0.866025403784438));
#8698=DIRECTION('',(0.,-1.,0.));
#8699=DIRECTION('',(0.5,0.,-0.866025403784438));
#8700=DIRECTION('center_axis',(-0.866025403784439,0.,0.5));
#8701=DIRECTION('ref_axis',(-0.5,0.,-0.866025403784439));
#8702=DIRECTION('',(0.5,0.,0.866025403784439));
#8703=DIRECTION('',(0.,-1.,0.));
#8704=DIRECTION('',(-0.5,0.,-0.866025403784439));
#8705=DIRECTION('center_axis',(-1.92296268638356E-16,0.,1.));
#8706=DIRECTION('ref_axis',(-1.,0.,-1.92296268638356E-16));
#8707=DIRECTION('',(1.,0.,1.92296268638356E-16));
#8708=DIRECTION('',(0.,-1.,0.));
#8709=DIRECTION('',(-1.,0.,-1.92296268638356E-16));
#8710=DIRECTION('center_axis',(0.866025403784439,0.,0.5));
#8711=DIRECTION('ref_axis',(-0.5,0.,0.866025403784439));
#8712=DIRECTION('',(0.5,0.,-0.866025403784439));
#8713=DIRECTION('',(-0.5,0.,0.866025403784439));
#8714=DIRECTION('center_axis',(0.,1.,0.));
#8715=DIRECTION('ref_axis',(1.,0.,0.));
#8716=DIRECTION('center_axis',(0.,-1.,0.));
#8717=DIRECTION('ref_axis',(0.,0.,-1.));
#8718=DIRECTION('axis',(0.,0.,1.));
#8719=DIRECTION('refdir',(1.,0.,0.));
#8720=DIRECTION('center_axis',(0.,1.,0.));
#8721=DIRECTION('ref_axis',(0.,0.,1.));
#8722=DIRECTION('center_axis',(0.,-1.,0.));
#8723=DIRECTION('ref_axis',(1.,0.,0.));
#8724=DIRECTION('center_axis',(0.,-1.,0.));
#8725=DIRECTION('ref_axis',(1.,0.,0.));
#8726=DIRECTION('center_axis',(0.,-1.,0.));
#8727=DIRECTION('ref_axis',(1.,0.,0.));
#8728=DIRECTION('',(0.707106781186547,0.707106781186548,8.65956056235493E-17));
#8729=DIRECTION('center_axis',(0.,-1.,0.));
#8730=DIRECTION('ref_axis',(1.,0.,0.));
#8731=DIRECTION('center_axis',(0.,-1.,0.));
#8732=DIRECTION('ref_axis',(1.,0.,0.));
#8733=DIRECTION('',(0.,1.,0.));
#8734=DIRECTION('center_axis',(0.,1.,0.));
#8735=DIRECTION('ref_axis',(1.,0.,0.));
#8736=DIRECTION('center_axis',(0.,-1.,0.));
#8737=DIRECTION('ref_axis',(1.,0.,0.));
#8738=DIRECTION('',(-0.707106781186547,0.707106781186548,-8.65956056235493E-17));
#8739=DIRECTION('center_axis',(0.,-1.,0.));
#8740=DIRECTION('ref_axis',(0.,0.,-1.));
#8741=DIRECTION('center_axis',(0.,-1.,0.));
#8742=DIRECTION('ref_axis',(1.,0.,0.));
#8743=DIRECTION('center_axis',(0.,1.,0.));
#8744=DIRECTION('ref_axis',(1.,0.,0.));
#8745=DIRECTION('center_axis',(0.,1.,0.));
#8746=DIRECTION('ref_axis',(1.,0.,0.));
#8747=DIRECTION('',(-0.447213595499958,0.894427190999916,-5.47678698264203E-17));
#8748=DIRECTION('center_axis',(0.,-1.,0.));
#8749=DIRECTION('ref_axis',(1.,0.,0.));
#8750=DIRECTION('center_axis',(0.,1.,0.));
#8751=DIRECTION('ref_axis',(1.,0.,0.));
#8752=DIRECTION('',(0.,1.,0.));
#8753=DIRECTION('center_axis',(0.,1.,0.));
#8754=DIRECTION('ref_axis',(1.,0.,0.));
#8755=DIRECTION('center_axis',(0.,-1.,0.));
#8756=DIRECTION('ref_axis',(1.,0.,0.));
#8757=DIRECTION('',(-0.707106781186547,0.707106781186548,-8.65956056235493E-17));
#8758=DIRECTION('center_axis',(0.,-1.,0.));
#8759=DIRECTION('ref_axis',(0.,0.,-1.));
#8760=DIRECTION('center_axis',(0.866025403784439,0.,-0.5));
#8761=DIRECTION('ref_axis',(0.5,0.,0.866025403784439));
#8762=DIRECTION('',(-0.5,0.,-0.866025403784439));
#8763=DIRECTION('',(0.,-1.,0.));
#8764=DIRECTION('',(0.5,0.,0.866025403784439));
#8765=DIRECTION('',(0.,-1.,0.));
#8766=DIRECTION('center_axis',(1.60246890531964E-16,0.,-1.));
#8767=DIRECTION('ref_axis',(1.,0.,1.60246890531964E-16));
#8768=DIRECTION('',(-1.,0.,-1.60246890531964E-16));
#8769=DIRECTION('',(0.,-1.,0.));
#8770=DIRECTION('',(1.,0.,1.60246890531964E-16));
#8771=DIRECTION('center_axis',(-0.866025403784439,0.,-0.5));
#8772=DIRECTION('ref_axis',(0.5,0.,-0.866025403784439));
#8773=DIRECTION('',(-0.5,0.,0.866025403784439));
#8774=DIRECTION('',(0.,-1.,0.));
#8775=DIRECTION('',(0.5,0.,-0.866025403784439));
#8776=DIRECTION('center_axis',(-0.866025403784439,0.,0.5));
#8777=DIRECTION('ref_axis',(-0.5,0.,-0.866025403784439));
#8778=DIRECTION('',(0.5,0.,0.866025403784439));
#8779=DIRECTION('',(0.,-1.,0.));
#8780=DIRECTION('',(-0.5,0.,-0.866025403784439));
#8781=DIRECTION('center_axis',(-1.60246890531964E-16,0.,1.));
#8782=DIRECTION('ref_axis',(-1.,0.,-1.60246890531964E-16));
#8783=DIRECTION('',(1.,0.,1.60246890531964E-16));
#8784=DIRECTION('',(0.,-1.,0.));
#8785=DIRECTION('',(-1.,0.,-1.60246890531964E-16));
#8786=DIRECTION('center_axis',(0.866025403784439,0.,0.5));
#8787=DIRECTION('ref_axis',(-0.5,0.,0.866025403784439));
#8788=DIRECTION('',(0.5,0.,-0.866025403784439));
#8789=DIRECTION('',(-0.5,0.,0.866025403784439));
#8790=DIRECTION('center_axis',(0.,1.,0.));
#8791=DIRECTION('ref_axis',(1.,0.,0.));
#8792=DIRECTION('center_axis',(0.,-1.,0.));
#8793=DIRECTION('ref_axis',(0.,0.,-1.));
#8794=DIRECTION('',(0.,0.,1.));
#8795=DIRECTION('',(1.,0.,0.));
#8796=DIRECTION('',(0.,0.,1.));
#8797=DIRECTION('',(1.,0.,0.));
#8798=DIRECTION('',(0.,0.,1.));
#8799=DIRECTION('',(1.,0.,0.));
#8800=DIRECTION('',(0.,0.,1.));
#8801=DIRECTION('',(1.,0.,0.));
#8802=DIRECTION('',(0.,0.,1.));
#8803=DIRECTION('',(1.,0.,0.));
#8804=DIRECTION('',(0.,0.,1.));
#8805=DIRECTION('',(1.,0.,0.));
#8806=DIRECTION('',(0.,0.,1.));
#8807=DIRECTION('',(1.,0.,0.));
#8808=DIRECTION('',(0.,0.,1.));
#8809=DIRECTION('',(1.,0.,0.));
#8810=DIRECTION('',(0.,-1.,2.22044604925031E-16));
#8811=DIRECTION('',(1.,0.,0.));
#8812=DIRECTION('',(0.,-1.,2.22044604925031E-16));
#8813=DIRECTION('',(1.,0.,0.));
#8814=DIRECTION('',(0.,0.,1.));
#8815=DIRECTION('',(1.,0.,0.));
#8816=DIRECTION('',(0.,-1.,2.22044604925031E-16));
#8817=DIRECTION('',(1.,0.,0.));
#8818=DIRECTION('',(0.,-1.,2.22044604925031E-16));
#8819=DIRECTION('',(1.,0.,0.));
#8820=DIRECTION('',(0.,0.,1.));
#8821=DIRECTION('',(-1.,1.22464679914735E-16,0.));
#8822=DIRECTION('',(0.,0.,1.));
#8823=DIRECTION('',(-1.,1.22464679914735E-16,0.));
#8824=DIRECTION('',(0.,0.,1.));
#8825=DIRECTION('',(-1.,1.22464679914735E-16,0.));
#8826=DIRECTION('',(0.,0.,1.));
#8827=DIRECTION('',(-1.,1.22464679914735E-16,0.));
#8828=DIRECTION('',(0.,0.,1.));
#8829=DIRECTION('',(1.,0.,0.));
#8830=DIRECTION('',(0.,0.,1.));
#8831=DIRECTION('',(1.,0.,0.));
#8832=DIRECTION('',(0.,0.,1.));
#8833=DIRECTION('',(1.,0.,0.));
#8834=DIRECTION('',(0.,0.,1.));
#8835=DIRECTION('',(1.,0.,0.));
#8836=DIRECTION('axis',(0.,0.,1.));
#8837=DIRECTION('refdir',(1.,0.,0.));
#8838=DIRECTION('axis',(0.,0.,1.));
#8839=DIRECTION('refdir',(1.,0.,0.));
#8840=DIRECTION('center_axis',(-1.,0.,0.));
#8841=DIRECTION('ref_axis',(0.,0.,1.));
#8842=DIRECTION('',(0.,-1.,0.));
#8843=DIRECTION('',(0.,0.,1.));
#8844=DIRECTION('',(0.,1.,0.));
#8845=DIRECTION('',(0.,0.,-1.));
#8846=DIRECTION('center_axis',(0.,1.,0.));
#8847=DIRECTION('ref_axis',(1.,0.,0.));
#8848=DIRECTION('center_axis',(0.,-1.,0.));
#8849=DIRECTION('ref_axis',(1.,0.,0.));
#8850=DIRECTION('',(-1.,0.,0.));
#8851=DIRECTION('',(0.,0.,1.));
#8852=DIRECTION('center_axis',(1.,0.,0.));
#8853=DIRECTION('ref_axis',(0.,0.,-1.));
#8854=DIRECTION('',(0.,1.,0.));
#8855=DIRECTION('',(0.,1.,0.));
#8856=DIRECTION('',(0.,0.,-1.));
#8857=DIRECTION('center_axis',(0.,0.,1.));
#8858=DIRECTION('ref_axis',(1.,0.,0.));
#8859=DIRECTION('',(1.,0.,0.));
#8860=DIRECTION('center_axis',(0.,1.,0.));
#8861=DIRECTION('ref_axis',(0.,0.,1.));
#8862=DIRECTION('center_axis',(0.,1.,0.));
#8863=DIRECTION('ref_axis',(1.,0.,0.));
#8864=DIRECTION('center_axis',(-1.,0.,0.));
#8865=DIRECTION('ref_axis',(0.,0.,1.));
#8866=DIRECTION('',(0.,-1.,0.));
#8867=DIRECTION('',(0.,0.,1.));
#8868=DIRECTION('',(0.,1.,0.));
#8869=DIRECTION('',(0.,0.,-1.));
#8870=DIRECTION('center_axis',(0.,1.,0.));
#8871=DIRECTION('ref_axis',(1.,0.,0.));
#8872=DIRECTION('center_axis',(0.,-1.,0.));
#8873=DIRECTION('ref_axis',(1.,0.,0.));
#8874=DIRECTION('',(-1.,0.,0.));
#8875=DIRECTION('',(0.,0.,1.));
#8876=DIRECTION('center_axis',(1.,0.,0.));
#8877=DIRECTION('ref_axis',(0.,0.,-1.));
#8878=DIRECTION('',(0.,1.,0.));
#8879=DIRECTION('',(0.,1.,0.));
#8880=DIRECTION('',(0.,0.,-1.));
#8881=DIRECTION('center_axis',(0.,0.,1.));
#8882=DIRECTION('ref_axis',(1.,0.,0.));
#8883=DIRECTION('',(1.,0.,0.));
#8884=DIRECTION('center_axis',(0.,1.,0.));
#8885=DIRECTION('ref_axis',(0.,0.,1.));
#8886=DIRECTION('center_axis',(0.,1.,0.));
#8887=DIRECTION('ref_axis',(1.,0.,0.));
#8888=DIRECTION('center_axis',(0.,1.,0.));
#8889=DIRECTION('ref_axis',(1.,0.,0.));
#8890=DIRECTION('center_axis',(0.,1.,0.));
#8891=DIRECTION('ref_axis',(1.,0.,0.));
#8892=DIRECTION('center_axis',(0.,1.,0.));
#8893=DIRECTION('ref_axis',(1.,0.,0.));
#8894=DIRECTION('center_axis',(0.,1.,0.));
#8895=DIRECTION('ref_axis',(1.,0.,0.));
#8896=DIRECTION('center_axis',(0.,1.,0.));
#8897=DIRECTION('ref_axis',(1.,0.,0.));
#8898=DIRECTION('center_axis',(0.,-1.,0.));
#8899=DIRECTION('ref_axis',(1.,0.,0.));
#8900=DIRECTION('center_axis',(0.,1.,0.));
#8901=DIRECTION('ref_axis',(1.,0.,0.));
#8902=DIRECTION('',(0.,-1.,0.));
#8903=DIRECTION('center_axis',(0.,1.,0.));
#8904=DIRECTION('ref_axis',(1.,0.,0.));
#8905=DIRECTION('',(0.,-1.,0.));
#8906=DIRECTION('center_axis',(0.,1.,0.));
#8907=DIRECTION('ref_axis',(1.,0.,0.));
#8908=DIRECTION('center_axis',(0.,1.,0.));
#8909=DIRECTION('ref_axis',(1.,0.,0.));
#8910=DIRECTION('center_axis',(0.,1.,0.));
#8911=DIRECTION('ref_axis',(1.,0.,0.));
#8912=DIRECTION('',(0.,-1.,0.));
#8913=DIRECTION('center_axis',(0.,1.,0.));
#8914=DIRECTION('ref_axis',(1.,0.,0.));
#8915=DIRECTION('center_axis',(0.,1.,0.));
#8916=DIRECTION('ref_axis',(1.,0.,0.));
#8917=DIRECTION('axis',(0.,0.,1.));
#8918=DIRECTION('refdir',(1.,0.,0.));
#8919=DIRECTION('center_axis',(0.,1.,0.));
#8920=DIRECTION('ref_axis',(1.,0.,0.));
#8921=DIRECTION('center_axis',(0.,-1.,0.));
#8922=DIRECTION('ref_axis',(1.,0.,0.));
#8923=DIRECTION('',(0.,-1.,0.));
#8924=DIRECTION('center_axis',(0.,-1.,0.));
#8925=DIRECTION('ref_axis',(1.,0.,0.));
#8926=DIRECTION('center_axis',(0.,1.,0.));
#8927=DIRECTION('ref_axis',(1.,0.,0.));
#8928=DIRECTION('center_axis',(0.,1.,0.));
#8929=DIRECTION('ref_axis',(1.,0.,0.));
#8930=DIRECTION('',(0.,-1.,0.));
#8931=DIRECTION('center_axis',(0.,1.,0.));
#8932=DIRECTION('ref_axis',(1.,0.,0.));
#8933=DIRECTION('center_axis',(0.,1.,0.));
#8934=DIRECTION('ref_axis',(1.,0.,0.));
#8935=DIRECTION('center_axis',(0.,1.,0.));
#8936=DIRECTION('ref_axis',(1.,0.,0.));
#8937=DIRECTION('axis',(0.,0.,1.));
#8938=DIRECTION('refdir',(1.,0.,0.));
#8939=DIRECTION('center_axis',(0.,0.,1.));
#8940=DIRECTION('ref_axis',(1.,0.,0.));
#8941=DIRECTION('',(0.,1.,0.));
#8942=DIRECTION('center_axis',(0.,0.,1.));
#8943=DIRECTION('ref_axis',(1.,0.,0.));
#8944=DIRECTION('center_axis',(0.,0.,1.));
#8945=DIRECTION('ref_axis',(1.,0.,0.));
#8946=DIRECTION('center_axis',(0.,0.,1.));
#8947=DIRECTION('ref_axis',(1.,0.,0.));
#8948=DIRECTION('',(0.,0.,1.));
#8949=DIRECTION('center_axis',(0.,0.,1.));
#8950=DIRECTION('ref_axis',(1.,0.,0.));
#8951=DIRECTION('center_axis',(0.,0.,1.));
#8952=DIRECTION('ref_axis',(1.,0.,0.));
#8953=DIRECTION('',(0.,-1.,0.));
#8954=DIRECTION('center_axis',(0.,1.,0.));
#8955=DIRECTION('ref_axis',(1.,0.,0.));
#8956=DIRECTION('center_axis',(0.,-1.,0.));
#8957=DIRECTION('ref_axis',(1.,0.,0.));
#8958=DIRECTION('',(0.,-1.,0.));
#8959=DIRECTION('center_axis',(0.,-1.,0.));
#8960=DIRECTION('ref_axis',(1.,0.,0.));
#8961=DIRECTION('center_axis',(0.,1.,0.));
#8962=DIRECTION('ref_axis',(1.,0.,0.));
#8963=DIRECTION('center_axis',(0.,1.,0.));
#8964=DIRECTION('ref_axis',(1.,0.,0.));
#8965=DIRECTION('',(0.,-1.,0.));
#8966=DIRECTION('center_axis',(0.,1.,0.));
#8967=DIRECTION('ref_axis',(1.,0.,0.));
#8968=DIRECTION('center_axis',(0.,1.,0.));
#8969=DIRECTION('ref_axis',(1.,0.,0.));
#8970=DIRECTION('center_axis',(0.,1.,0.));
#8971=DIRECTION('ref_axis',(1.,0.,0.));
#8972=DIRECTION('axis',(0.,0.,1.));
#8973=DIRECTION('refdir',(1.,0.,0.));
#8974=DIRECTION('center_axis',(0.,0.,1.));
#8975=DIRECTION('ref_axis',(1.,0.,0.));
#8976=DIRECTION('',(0.,1.,0.));
#8977=DIRECTION('center_axis',(0.,0.,1.));
#8978=DIRECTION('ref_axis',(1.,0.,0.));
#8979=DIRECTION('center_axis',(0.,0.,1.));
#8980=DIRECTION('ref_axis',(1.,0.,0.));
#8981=DIRECTION('center_axis',(0.,0.,1.));
#8982=DIRECTION('ref_axis',(1.,0.,0.));
#8983=DIRECTION('',(0.,0.,1.));
#8984=DIRECTION('center_axis',(0.,0.,1.));
#8985=DIRECTION('ref_axis',(1.,0.,0.));
#8986=DIRECTION('center_axis',(0.,0.,1.));
#8987=DIRECTION('ref_axis',(1.,0.,0.));
#8988=DIRECTION('',(0.,-1.,0.));
#8989=DIRECTION('center_axis',(0.,0.,-1.));
#8990=DIRECTION('ref_axis',(-1.,0.,0.));
#8991=DIRECTION('',(1.,0.,0.));
#8992=DIRECTION('',(0.,1.,0.));
#8993=DIRECTION('',(1.,0.,0.));
#8994=DIRECTION('',(0.,1.,0.));
#8995=DIRECTION('center_axis',(1.,0.,0.));
#8996=DIRECTION('ref_axis',(0.,0.,-1.));
#8997=DIRECTION('',(0.,0.,1.));
#8998=DIRECTION('',(0.,0.,1.));
#8999=DIRECTION('',(0.,1.,0.));
#9000=DIRECTION('',(0.,0.,1.));
#9001=DIRECTION('',(0.,-1.,0.));
#9002=DIRECTION('center_axis',(-1.,0.,0.));
#9003=DIRECTION('ref_axis',(0.,0.,1.));
#9004=DIRECTION('',(0.,0.,-1.));
#9005=DIRECTION('',(0.,1.,0.));
#9006=DIRECTION('',(0.,0.,-1.));
#9007=DIRECTION('',(0.,1.,0.));
#9008=DIRECTION('',(0.,0.,-1.));
#9009=DIRECTION('center_axis',(0.,0.,1.));
#9010=DIRECTION('ref_axis',(1.,0.,0.));
#9011=DIRECTION('',(-1.,0.,0.));
#9012=DIRECTION('',(-1.,0.,0.));
#9013=DIRECTION('center_axis',(0.,1.,0.));
#9014=DIRECTION('ref_axis',(1.,0.,0.));
#9015=DIRECTION('center_axis',(0.,1.,0.));
#9016=DIRECTION('ref_axis',(1.,0.,0.));
#9017=DIRECTION('center_axis',(0.,1.,0.));
#9018=DIRECTION('ref_axis',(1.,0.,0.));
#9019=DIRECTION('center_axis',(0.,-1.,0.));
#9020=DIRECTION('ref_axis',(1.,0.,0.));
#9021=DIRECTION('center_axis',(-1.,0.,0.));
#9022=DIRECTION('ref_axis',(0.,0.,1.));
#9023=DIRECTION('',(0.,0.,-1.));
#9024=DIRECTION('',(0.,1.,0.));
#9025=DIRECTION('',(0.,0.,1.));
#9026=DIRECTION('',(0.,1.,0.));
#9027=DIRECTION('center_axis',(0.,0.,-1.));
#9028=DIRECTION('ref_axis',(-1.,0.,0.));
#9029=DIRECTION('',(1.,0.,0.));
#9030=DIRECTION('',(-1.,0.,0.));
#9031=DIRECTION('',(0.,1.,0.));
#9032=DIRECTION('center_axis',(1.,0.,0.));
#9033=DIRECTION('ref_axis',(0.,0.,-1.));
#9034=DIRECTION('',(0.,0.,1.));
#9035=DIRECTION('',(0.,0.,-1.));
#9036=DIRECTION('',(0.,1.,0.));
#9037=DIRECTION('center_axis',(0.,0.,1.));
#9038=DIRECTION('ref_axis',(1.,0.,0.));
#9039=DIRECTION('',(-1.,0.,0.));
#9040=DIRECTION('',(1.,0.,0.));
#9041=DIRECTION('center_axis',(0.,1.,0.));
#9042=DIRECTION('ref_axis',(1.,0.,0.));
#9043=DIRECTION('center_axis',(0.,1.,0.));
#9044=DIRECTION('ref_axis',(1.,0.,0.));
#9045=DIRECTION('center_axis',(0.,-1.,0.));
#9046=DIRECTION('ref_axis',(1.,0.,0.));
#9047=DIRECTION('center_axis',(0.,1.,0.));
#9048=DIRECTION('ref_axis',(1.,0.,0.));
#9049=DIRECTION('center_axis',(0.,1.,0.));
#9050=DIRECTION('ref_axis',(1.,0.,0.));
#9051=DIRECTION('center_axis',(0.,1.,0.));
#9052=DIRECTION('ref_axis',(-1.83697019872103E-16,0.,1.));
#9053=DIRECTION('center_axis',(0.,1.,0.));
#9054=DIRECTION('ref_axis',(1.,0.,0.));
#9055=DIRECTION('',(0.,-1.,0.));
#9056=DIRECTION('axis',(0.,0.,1.));
#9057=DIRECTION('refdir',(1.,0.,0.));
#9058=DIRECTION('center_axis',(0.,0.,1.));
#9059=DIRECTION('ref_axis',(1.,0.,0.));
#9060=DIRECTION('',(0.,1.,0.));
#9061=DIRECTION('center_axis',(0.,0.,1.));
#9062=DIRECTION('ref_axis',(1.,0.,0.));
#9063=DIRECTION('center_axis',(0.,0.,1.));
#9064=DIRECTION('ref_axis',(1.,0.,0.));
#9065=DIRECTION('center_axis',(0.,0.,1.));
#9066=DIRECTION('ref_axis',(1.,0.,0.));
#9067=DIRECTION('',(0.,0.,1.));
#9068=DIRECTION('center_axis',(0.,0.,1.));
#9069=DIRECTION('ref_axis',(1.,0.,0.));
#9070=DIRECTION('center_axis',(0.,0.,1.));
#9071=DIRECTION('ref_axis',(1.,0.,0.));
#9072=DIRECTION('',(0.,-1.,0.));
#9073=DIRECTION('center_axis',(-1.,0.,0.));
#9074=DIRECTION('ref_axis',(0.,0.,1.));
#9075=DIRECTION('',(0.,0.,1.));
#9076=DIRECTION('',(0.,1.,0.));
#9077=DIRECTION('',(0.,0.,-1.));
#9078=DIRECTION('',(0.,1.,0.));
#9079=DIRECTION('center_axis',(0.,0.,-1.));
#9080=DIRECTION('ref_axis',(-1.,0.,0.));
#9081=DIRECTION('',(-1.,0.,0.));
#9082=DIRECTION('',(0.,1.,0.));
#9083=DIRECTION('',(1.,0.,0.));
#9084=DIRECTION('center_axis',(1.,0.,0.));
#9085=DIRECTION('ref_axis',(0.,0.,-1.));
#9086=DIRECTION('',(0.,0.,-1.));
#9087=DIRECTION('',(0.,-1.,0.));
#9088=DIRECTION('',(0.,0.,1.));
#9089=DIRECTION('center_axis',(0.,1.,0.));
#9090=DIRECTION('ref_axis',(1.,0.,0.));
#9091=DIRECTION('center_axis',(0.,1.,0.));
#9092=DIRECTION('ref_axis',(1.,0.,0.));
#9093=DIRECTION('center_axis',(0.,-1.,0.));
#9094=DIRECTION('ref_axis',(1.,0.,0.));
#9095=DIRECTION('center_axis',(0.,1.,0.));
#9096=DIRECTION('ref_axis',(-1.83697019872103E-16,0.,1.));
#9097=DIRECTION('center_axis',(0.,-1.,0.));
#9098=DIRECTION('ref_axis',(1.,0.,0.));
#9099=DIRECTION('center_axis',(0.,1.,0.));
#9100=DIRECTION('ref_axis',(1.,0.,0.));
#9101=DIRECTION('center_axis',(0.,1.,0.));
#9102=DIRECTION('ref_axis',(1.,0.,0.));
#9103=DIRECTION('',(0.,1.,0.));
#9104=DIRECTION('center_axis',(0.,-1.,0.));
#9105=DIRECTION('ref_axis',(1.,0.,0.));
#9106=DIRECTION('center_axis',(0.,1.,0.));
#9107=DIRECTION('ref_axis',(1.,0.,0.));
#9108=DIRECTION('',(0.,-1.,0.));
#9109=DIRECTION('center_axis',(0.,1.,0.));
#9110=DIRECTION('ref_axis',(1.,0.,0.));
#9111=DIRECTION('',(0.,1.,0.));
#9112=DIRECTION('center_axis',(0.,1.,0.));
#9113=DIRECTION('ref_axis',(1.,0.,0.));
#9114=DIRECTION('center_axis',(0.,1.,0.));
#9115=DIRECTION('ref_axis',(1.,0.,0.));
#9116=DIRECTION('',(-1.,0.,0.));
#9117=DIRECTION('center_axis',(0.,-1.,0.));
#9118=DIRECTION('ref_axis',(1.,0.,0.));
#9119=DIRECTION('',(1.,0.,0.));
#9120=DIRECTION('center_axis',(0.,0.,1.));
#9121=DIRECTION('ref_axis',(1.,0.,0.));
#9122=DIRECTION('',(1.,0.,0.));
#9123=DIRECTION('',(0.,1.,0.));
#9124=DIRECTION('center_axis',(0.,1.,0.));
#9125=DIRECTION('ref_axis',(0.,0.,1.));
#9126=DIRECTION('',(-1.,0.,0.));
#9127=DIRECTION('center_axis',(0.,1.,0.));
#9128=DIRECTION('ref_axis',(1.,0.,0.));
#9129=DIRECTION('center_axis',(0.,0.,-1.));
#9130=DIRECTION('ref_axis',(-1.,0.,0.));
#9131=DIRECTION('',(0.,-1.,0.));
#9132=DIRECTION('center_axis',(0.,1.,0.));
#9133=DIRECTION('ref_axis',(1.,0.,0.));
#9134=DIRECTION('',(0.,-1.,0.));
#9135=DIRECTION('center_axis',(0.,1.,0.));
#9136=DIRECTION('ref_axis',(1.,0.,0.));
#9137=DIRECTION('center_axis',(0.,1.,0.));
#9138=DIRECTION('ref_axis',(1.,0.,0.));
#9139=DIRECTION('axis',(0.,0.,1.));
#9140=DIRECTION('refdir',(1.,0.,0.));
#9141=DIRECTION('center_axis',(0.,1.,0.));
#9142=DIRECTION('ref_axis',(1.,0.,0.));
#9143=DIRECTION('center_axis',(0.,1.,0.));
#9144=DIRECTION('ref_axis',(1.,0.,0.));
#9145=DIRECTION('',(0.,-1.,0.));
#9146=DIRECTION('center_axis',(0.,-1.,0.));
#9147=DIRECTION('ref_axis',(1.,0.,0.));
#9148=DIRECTION('center_axis',(0.,1.,0.));
#9149=DIRECTION('ref_axis',(1.,0.,0.));
#9150=DIRECTION('center_axis',(0.,-1.,0.));
#9151=DIRECTION('ref_axis',(1.,0.,0.));
#9152=DIRECTION('center_axis',(0.,1.,0.));
#9153=DIRECTION('ref_axis',(1.,0.,0.));
#9154=DIRECTION('',(0.,-1.,0.));
#9155=DIRECTION('center_axis',(0.,-1.,0.));
#9156=DIRECTION('ref_axis',(1.,0.,0.));
#9157=DIRECTION('center_axis',(0.,1.,0.));
#9158=DIRECTION('ref_axis',(1.,0.,0.));
#9159=DIRECTION('center_axis',(0.,1.,0.));
#9160=DIRECTION('ref_axis',(1.,0.,0.));
#9161=DIRECTION('',(0.,-1.,0.));
#9162=DIRECTION('center_axis',(0.,1.,0.));
#9163=DIRECTION('ref_axis',(1.,0.,0.));
#9164=DIRECTION('center_axis',(0.,1.,0.));
#9165=DIRECTION('ref_axis',(1.,0.,0.));
#9166=DIRECTION('center_axis',(0.,1.,0.));
#9167=DIRECTION('ref_axis',(1.,0.,0.));
#9168=DIRECTION('axis',(0.,0.,1.));
#9169=DIRECTION('refdir',(1.,0.,0.));
#9170=DIRECTION('center_axis',(0.,1.,0.));
#9171=DIRECTION('ref_axis',(1.,0.,0.));
#9172=DIRECTION('center_axis',(0.,1.,0.));
#9173=DIRECTION('ref_axis',(1.,0.,0.));
#9174=DIRECTION('',(0.,-1.,0.));
#9175=DIRECTION('center_axis',(0.,1.,0.));
#9176=DIRECTION('ref_axis',(1.,0.,0.));
#9177=DIRECTION('center_axis',(0.,1.,0.));
#9178=DIRECTION('ref_axis',(1.,0.,0.));
#9179=DIRECTION('center_axis',(0.,-1.,0.));
#9180=DIRECTION('ref_axis',(1.,0.,0.));
#9181=DIRECTION('center_axis',(0.,1.,0.));
#9182=DIRECTION('ref_axis',(1.,0.,0.));
#9183=DIRECTION('center_axis',(0.,-1.,0.));
#9184=DIRECTION('ref_axis',(1.,0.,0.));
#9185=DIRECTION('',(0.,-1.,0.));
#9186=DIRECTION('center_axis',(0.,1.,0.));
#9187=DIRECTION('ref_axis',(1.,0.,0.));
#9188=DIRECTION('center_axis',(0.,1.,0.));
#9189=DIRECTION('ref_axis',(1.,0.,0.));
#9190=DIRECTION('',(0.,-1.,0.));
#9191=DIRECTION('center_axis',(0.,1.,0.));
#9192=DIRECTION('ref_axis',(1.,0.,0.));
#9193=DIRECTION('center_axis',(0.,1.,0.));
#9194=DIRECTION('ref_axis',(1.,0.,0.));
#9195=DIRECTION('center_axis',(0.,1.,0.));
#9196=DIRECTION('ref_axis',(1.,0.,0.));
#9197=DIRECTION('axis',(0.,0.,1.));
#9198=DIRECTION('refdir',(1.,0.,0.));
#9199=DIRECTION('center_axis',(1.,0.,0.));
#9200=DIRECTION('ref_axis',(0.,0.,-1.));
#9201=DIRECTION('',(0.,0.707106781186548,-0.707106781186548));
#9202=DIRECTION('',(0.,1.,0.));
#9203=DIRECTION('',(0.,0.707106781186548,0.707106781186548));
#9204=DIRECTION('',(0.,0.,1.));
#9205=DIRECTION('',(0.,-0.707106781186548,0.707106781186547));
#9206=DIRECTION('',(0.,-1.,0.));
#9207=DIRECTION('',(0.,-0.707106781186548,-0.707106781186547));
#9208=DIRECTION('',(0.,0.,-1.));
#9209=DIRECTION('center_axis',(0.,-0.707106781186547,-0.707106781186548));
#9210=DIRECTION('ref_axis',(-1.,0.,0.));
#9211=DIRECTION('',(-1.,0.,0.));
#9212=DIRECTION('',(0.,0.707106781186548,-0.707106781186547));
#9213=DIRECTION('',(1.,0.,0.));
#9214=DIRECTION('center_axis',(0.,-1.,0.));
#9215=DIRECTION('ref_axis',(1.,0.,0.));
#9216=DIRECTION('',(1.,0.,0.));
#9217=DIRECTION('',(0.,0.,-1.));
#9218=DIRECTION('center_axis',(0.,-0.707106781186548,0.707106781186548));
#9219=DIRECTION('ref_axis',(1.,0.,0.));
#9220=DIRECTION('',(-1.,0.,0.));
#9221=DIRECTION('',(0.,-0.707106781186548,-0.707106781186548));
#9222=DIRECTION('center_axis',(0.,0.,1.));
#9223=DIRECTION('ref_axis',(1.,0.,0.));
#9224=DIRECTION('',(1.,0.,0.));
#9225=DIRECTION('',(0.,-1.,0.));
#9226=DIRECTION('center_axis',(1.,0.,0.));
#9227=DIRECTION('ref_axis',(0.,0.,-1.));
#9228=DIRECTION('',(0.,-0.707106781186548,0.707106781186548));
#9229=DIRECTION('',(0.,0.,1.));
#9230=DIRECTION('',(0.,0.707106781186548,0.707106781186547));
#9231=DIRECTION('',(0.,1.,0.));
#9232=DIRECTION('center_axis',(0.,0.707106781186548,0.707106781186548));
#9233=DIRECTION('ref_axis',(1.,0.,0.));
#9234=DIRECTION('',(-1.,0.,0.));
#9235=DIRECTION('center_axis',(0.,1.,0.));
#9236=DIRECTION('ref_axis',(-1.,0.,0.));
#9237=DIRECTION('',(1.,0.,0.));
#9238=DIRECTION('center_axis',(0.,0.707106781186547,-0.707106781186548));
#9239=DIRECTION('ref_axis',(-1.,0.,0.));
#9240=DIRECTION('',(-1.,0.,0.));
#9241=DIRECTION('center_axis',(0.,0.,1.));
#9242=DIRECTION('ref_axis',(1.,0.,0.));
#9243=DIRECTION('axis',(0.,0.,1.));
#9244=DIRECTION('refdir',(1.,0.,0.));
#9245=DIRECTION('center_axis',(0.866025403784439,0.,-0.5));
#9246=DIRECTION('ref_axis',(0.5,0.,0.866025403784439));
#9247=DIRECTION('',(0.5,0.,0.866025403784439));
#9248=DIRECTION('',(0.,-1.,0.));
#9249=DIRECTION('',(0.5,0.,0.866025403784439));
#9250=DIRECTION('',(0.,-1.,0.));
#9251=DIRECTION('center_axis',(1.92296268638356E-16,0.,-1.));
#9252=DIRECTION('ref_axis',(1.,0.,1.92296268638356E-16));
#9253=DIRECTION('',(1.,0.,1.92296268638356E-16));
#9254=DIRECTION('',(0.,-1.,0.));
#9255=DIRECTION('',(1.,0.,1.92296268638356E-16));
#9256=DIRECTION('center_axis',(-0.866025403784439,0.,-0.5));
#9257=DIRECTION('ref_axis',(0.5,0.,-0.866025403784439));
#9258=DIRECTION('',(0.5,0.,-0.866025403784439));
#9259=DIRECTION('',(0.,-1.,0.));
#9260=DIRECTION('',(0.5,0.,-0.866025403784438));
#9261=DIRECTION('center_axis',(-0.866025403784439,0.,0.5));
#9262=DIRECTION('ref_axis',(-0.5,0.,-0.866025403784439));
#9263=DIRECTION('',(-0.5,0.,-0.866025403784439));
#9264=DIRECTION('',(0.,-1.,0.));
#9265=DIRECTION('',(-0.5,0.,-0.866025403784439));
#9266=DIRECTION('center_axis',(-1.92296268638356E-16,0.,1.));
#9267=DIRECTION('ref_axis',(-1.,0.,-1.92296268638356E-16));
#9268=DIRECTION('',(-1.,0.,-1.92296268638356E-16));
#9269=DIRECTION('',(0.,-1.,0.));
#9270=DIRECTION('',(-1.,0.,-1.92296268638356E-16));
#9271=DIRECTION('center_axis',(0.866025403784439,0.,0.5));
#9272=DIRECTION('ref_axis',(-0.5,0.,0.866025403784439));
#9273=DIRECTION('',(-0.5,0.,0.866025403784439));
#9274=DIRECTION('',(-0.5,0.,0.866025403784439));
#9275=DIRECTION('center_axis',(0.,-1.,0.));
#9276=DIRECTION('ref_axis',(0.,0.,-1.));
#9277=DIRECTION('center_axis',(0.,1.,0.));
#9278=DIRECTION('ref_axis',(0.,0.,1.));
#9279=DIRECTION('center_axis',(0.,-1.,0.));
#9280=DIRECTION('ref_axis',(1.,0.,0.));
#9281=DIRECTION('center_axis',(0.,-1.,0.));
#9282=DIRECTION('ref_axis',(1.,0.,0.));
#9283=DIRECTION('center_axis',(0.,-1.,0.));
#9284=DIRECTION('ref_axis',(1.,0.,0.));
#9285=DIRECTION('',(0.707106781186547,0.707106781186548,8.65956056235493E-17));
#9286=DIRECTION('center_axis',(0.,-1.,0.));
#9287=DIRECTION('ref_axis',(1.,0.,0.));
#9288=DIRECTION('center_axis',(0.,1.,0.));
#9289=DIRECTION('ref_axis',(1.,0.,0.));
#9290=DIRECTION('',(0.,1.,0.));
#9291=DIRECTION('center_axis',(0.,1.,0.));
#9292=DIRECTION('ref_axis',(1.,0.,0.));
#9293=DIRECTION('center_axis',(0.,-1.,0.));
#9294=DIRECTION('ref_axis',(1.,0.,0.));
#9295=DIRECTION('',(-0.707106781186547,0.707106781186548,-8.65956056235493E-17));
#9296=DIRECTION('center_axis',(0.,-1.,0.));
#9297=DIRECTION('ref_axis',(0.,0.,-1.));
#9298=DIRECTION('axis',(0.,0.,1.));
#9299=DIRECTION('refdir',(1.,0.,0.));
#9300=DIRECTION('axis',(0.,0.,1.));
#9301=DIRECTION('refdir',(1.,0.,0.));
#9302=DIRECTION('center_axis',(0.,-1.,0.));
#9303=DIRECTION('ref_axis',(0.,0.,-1.));
#9304=DIRECTION('center_axis',(0.,-1.,0.));
#9305=DIRECTION('ref_axis',(1.,0.,0.));
#9306=DIRECTION('center_axis',(0.,-1.,0.));
#9307=DIRECTION('ref_axis',(1.,0.,0.));
#9308=DIRECTION('center_axis',(1.,0.,1.22464679914735E-16));
#9309=DIRECTION('ref_axis',(-1.22464679914735E-16,0.,1.));
#9310=DIRECTION('center_axis',(0.,1.,0.));
#9311=DIRECTION('ref_axis',(1.,0.,0.));
#9312=DIRECTION('center_axis',(0.,1.,0.));
#9313=DIRECTION('ref_axis',(1.,0.,0.));
#9314=DIRECTION('center_axis',(0.,-1.,0.));
#9315=DIRECTION('ref_axis',(1.,0.,0.));
#9316=DIRECTION('',(0.,1.,0.));
#9317=DIRECTION('center_axis',(0.,-1.,0.));
#9318=DIRECTION('ref_axis',(1.,0.,0.));
#9319=DIRECTION('center_axis',(0.,-1.,0.));
#9320=DIRECTION('ref_axis',(1.,0.,0.));
#9321=DIRECTION('center_axis',(0.,-1.,0.));
#9322=DIRECTION('ref_axis',(1.,0.,0.));
#9323=DIRECTION('',(0.,1.,0.));
#9324=DIRECTION('center_axis',(0.,-1.,0.));
#9325=DIRECTION('ref_axis',(1.,0.,0.));
#9326=DIRECTION('center_axis',(0.,1.,0.));
#9327=DIRECTION('ref_axis',(1.,0.,0.));
#9328=DIRECTION('',(-0.707106781186547,0.707106781186548,-8.65956056235493E-17));
#9329=DIRECTION('center_axis',(0.,-1.,0.));
#9330=DIRECTION('ref_axis',(1.,0.,0.));
#9331=DIRECTION('center_axis',(0.,1.,0.));
#9332=DIRECTION('ref_axis',(0.,0.,1.));
#9333=DIRECTION('center_axis',(0.,-1.,0.));
#9334=DIRECTION('ref_axis',(1.,0.,0.));
#9335=DIRECTION('center_axis',(0.,-1.,0.));
#9336=DIRECTION('ref_axis',(1.,0.,0.));
#9337=DIRECTION('',(0.,1.,0.));
#9338=DIRECTION('center_axis',(0.,-1.,0.));
#9339=DIRECTION('ref_axis',(0.,0.,-1.));
#9340=DIRECTION('center_axis',(0.,-1.,0.));
#9341=DIRECTION('ref_axis',(1.,0.,0.));
#9342=DIRECTION('center_axis',(0.,-1.,0.));
#9343=DIRECTION('ref_axis',(1.,0.,0.));
#9344=DIRECTION('',(0.707106781186547,0.707106781186548,8.65956056235493E-17));
#9345=DIRECTION('axis',(0.,0.,1.));
#9346=DIRECTION('refdir',(1.,0.,0.));
#9347=DIRECTION('center_axis',(0.,-1.,0.));
#9348=DIRECTION('ref_axis',(0.,0.,-1.));
#9349=DIRECTION('center_axis',(0.,-1.,0.));
#9350=DIRECTION('ref_axis',(1.,0.,0.));
#9351=DIRECTION('center_axis',(0.,-1.,0.));
#9352=DIRECTION('ref_axis',(1.,0.,0.));
#9353=DIRECTION('center_axis',(1.,0.,1.22464679914735E-16));
#9354=DIRECTION('ref_axis',(-1.22464679914735E-16,0.,1.));
#9355=DIRECTION('center_axis',(0.,1.,0.));
#9356=DIRECTION('ref_axis',(1.,0.,0.));
#9357=DIRECTION('center_axis',(0.,1.,0.));
#9358=DIRECTION('ref_axis',(1.,0.,0.));
#9359=DIRECTION('center_axis',(0.,-1.,0.));
#9360=DIRECTION('ref_axis',(1.,0.,0.));
#9361=DIRECTION('center_axis',(0.,-1.,0.));
#9362=DIRECTION('ref_axis',(1.,0.,0.));
#9363=DIRECTION('',(0.,1.,0.));
#9364=DIRECTION('center_axis',(0.,1.,0.));
#9365=DIRECTION('ref_axis',(0.,0.,1.));
#9366=DIRECTION('center_axis',(0.,-1.,0.));
#9367=DIRECTION('ref_axis',(1.,0.,0.));
#9368=DIRECTION('center_axis',(0.,-1.,0.));
#9369=DIRECTION('ref_axis',(1.,0.,0.));
#9370=DIRECTION('center_axis',(0.,-1.,0.));
#9371=DIRECTION('ref_axis',(1.,0.,0.));
#9372=DIRECTION('center_axis',(0.,-1.,0.));
#9373=DIRECTION('ref_axis',(1.,0.,0.));
#9374=DIRECTION('',(0.707106781186548,0.707106781186547,8.65956056235494E-17));
#9375=DIRECTION('center_axis',(0.,-1.,0.));
#9376=DIRECTION('ref_axis',(1.,0.,0.));
#9377=DIRECTION('center_axis',(0.,-1.,0.));
#9378=DIRECTION('ref_axis',(1.,0.,0.));
#9379=DIRECTION('',(0.,1.,0.));
#9380=DIRECTION('center_axis',(0.,1.,0.));
#9381=DIRECTION('ref_axis',(1.,0.,0.));
#9382=DIRECTION('center_axis',(0.,-1.,0.));
#9383=DIRECTION('ref_axis',(1.,0.,0.));
#9384=DIRECTION('',(-0.707106781186548,0.707106781186547,-8.65956056235494E-17));
#9385=DIRECTION('center_axis',(0.,-1.,0.));
#9386=DIRECTION('ref_axis',(0.,0.,-1.));
#9387=DIRECTION('center_axis',(0.,-1.,0.));
#9388=DIRECTION('ref_axis',(1.,0.,0.));
#9389=DIRECTION('',(0.,1.,0.));
#9390=DIRECTION('axis',(0.,0.,1.));
#9391=DIRECTION('refdir',(1.,0.,0.));
#9392=DIRECTION('center_axis',(0.,0.,1.));
#9393=DIRECTION('ref_axis',(1.,0.,0.));
#9394=DIRECTION('center_axis',(1.22464679914735E-16,-1.,0.));
#9395=DIRECTION('ref_axis',(-1.,-1.22464679914735E-16,0.));
#9396=DIRECTION('center_axis',(0.707106781186548,0.,0.707106781186548));
#9397=DIRECTION('ref_axis',(0.707106781186548,0.,-0.707106781186548));
#9398=DIRECTION('center_axis',(8.65956056235494E-17,-1.,-8.65956056235493E-17));
#9399=DIRECTION('ref_axis',(-0.707106781186547,-1.22464679914735E-16,0.707106781186547));
#9400=DIRECTION('center_axis',(1.,0.,0.));
#9401=DIRECTION('ref_axis',(6.12323399573676E-17,0.,-1.));
#9402=DIRECTION('center_axis',(7.49879891330929E-33,-1.,-1.22464679914735E-16));
#9403=DIRECTION('ref_axis',(-6.12323399573676E-17,-1.22464679914735E-16,
1.));
#9404=DIRECTION('center_axis',(0.707106781186548,0.,-0.707106781186548));
#9405=DIRECTION('ref_axis',(-0.707106781186548,0.,-0.707106781186548));
#9406=DIRECTION('center_axis',(-8.65956056235493E-17,-1.,-8.65956056235494E-17));
#9407=DIRECTION('ref_axis',(0.707106781186547,-1.22464679914735E-16,0.707106781186547));
#9408=DIRECTION('center_axis',(0.,0.,-1.));
#9409=DIRECTION('ref_axis',(-1.,0.,-1.22464679914735E-16));
#9410=DIRECTION('center_axis',(-1.22464679914735E-16,-1.,-1.49975978266186E-32));
#9411=DIRECTION('ref_axis',(1.,-1.22464679914735E-16,1.22464679914735E-16));
#9412=DIRECTION('center_axis',(-0.707106781186547,0.,-0.707106781186548));
#9413=DIRECTION('ref_axis',(-0.707106781186548,0.,0.707106781186547));
#9414=DIRECTION('center_axis',(-8.65956056235493E-17,-1.,8.65956056235493E-17));
#9415=DIRECTION('ref_axis',(0.707106781186548,-1.22464679914735E-16,-0.707106781186547));
#9416=DIRECTION('center_axis',(-1.,0.,0.));
#9417=DIRECTION('ref_axis',(-1.83697019872103E-16,0.,1.));
#9418=DIRECTION('center_axis',(-2.24963967399279E-32,-1.,1.22464679914735E-16));
#9419=DIRECTION('ref_axis',(1.83697019872103E-16,-1.22464679914735E-16,
-1.));
#9420=DIRECTION('center_axis',(-0.707106781186548,0.,0.707106781186548));
#9421=DIRECTION('ref_axis',(0.707106781186547,0.,0.707106781186548));
#9422=DIRECTION('center_axis',(8.65956056235493E-17,-1.,8.65956056235493E-17));
#9423=DIRECTION('ref_axis',(-0.707106781186547,-1.22464679914735E-16,-0.707106781186548));
#9424=DIRECTION('axis',(0.,0.,1.));
#9425=DIRECTION('refdir',(1.,0.,0.));
#9426=DIRECTION('center_axis',(0.,0.,1.));
#9427=DIRECTION('ref_axis',(1.,0.,0.));
#9428=DIRECTION('center_axis',(0.,-1.,0.));
#9429=DIRECTION('ref_axis',(0.,0.,-1.));
#9430=DIRECTION('center_axis',(0.,-1.,0.));
#9431=DIRECTION('ref_axis',(0.,0.,-1.));
#9432=DIRECTION('center_axis',(0.,1.,0.));
#9433=DIRECTION('ref_axis',(1.,0.,0.));
#9434=DIRECTION('center_axis',(0.,1.,0.));
#9435=DIRECTION('ref_axis',(1.,0.,0.));
#9436=DIRECTION('center_axis',(0.,1.,0.));
#9437=DIRECTION('ref_axis',(1.,0.,0.));
#9438=DIRECTION('center_axis',(0.,1.,0.));
#9439=DIRECTION('ref_axis',(1.,0.,0.));
#9440=DIRECTION('',(0.,-1.,0.));
#9441=DIRECTION('center_axis',(0.,-1.,0.));
#9442=DIRECTION('ref_axis',(1.,0.,0.));
#9443=DIRECTION('center_axis',(0.,1.,0.));
#9444=DIRECTION('ref_axis',(1.,0.,0.));
#9445=DIRECTION('center_axis',(0.,1.,0.));
#9446=DIRECTION('ref_axis',(1.,0.,0.));
#9447=DIRECTION('center_axis',(0.,1.,0.));
#9448=DIRECTION('ref_axis',(1.,0.,0.));
#9449=DIRECTION('center_axis',(0.,1.,0.));
#9450=DIRECTION('ref_axis',(1.,0.,0.));
#9451=DIRECTION('center_axis',(0.,1.,0.));
#9452=DIRECTION('ref_axis',(1.,0.,0.));
#9453=DIRECTION('center_axis',(0.,1.,0.));
#9454=DIRECTION('ref_axis',(1.,0.,0.));
#9455=DIRECTION('center_axis',(0.,-1.,0.));
#9456=DIRECTION('ref_axis',(1.,0.,0.));
#9457=DIRECTION('center_axis',(0.,-1.,0.));
#9458=DIRECTION('ref_axis',(0.,0.,-1.));
#9459=DIRECTION('center_axis',(6.12323399573677E-17,0.,1.));
#9460=DIRECTION('ref_axis',(1.,0.,0.));
#9461=DIRECTION('center_axis',(0.,-1.,0.));
#9462=DIRECTION('ref_axis',(0.,0.,-1.));
#9463=DIRECTION('center_axis',(0.,1.,0.));
#9464=DIRECTION('ref_axis',(1.,0.,0.));
#9465=DIRECTION('center_axis',(0.,-1.,0.));
#9466=DIRECTION('ref_axis',(1.,0.,0.));
#9467=DIRECTION('center_axis',(0.,-1.,0.));
#9468=DIRECTION('ref_axis',(0.,0.,-1.));
#9469=DIRECTION('center_axis',(0.,0.,1.));
#9470=DIRECTION('ref_axis',(1.,0.,0.));
#9471=DIRECTION('center_axis',(0.,-1.,0.));
#9472=DIRECTION('ref_axis',(0.,0.,-1.));
#9473=DIRECTION('center_axis',(0.,1.,0.));
#9474=DIRECTION('ref_axis',(1.,0.,0.));
#9475=DIRECTION('center_axis',(0.,-1.,0.));
#9476=DIRECTION('ref_axis',(1.,0.,0.));
#9477=DIRECTION('center_axis',(0.,-1.,0.));
#9478=DIRECTION('ref_axis',(0.,0.,-1.));
#9479=DIRECTION('center_axis',(0.,0.,1.));
#9480=DIRECTION('ref_axis',(1.,0.,0.));
#9481=DIRECTION('center_axis',(0.,-1.,0.));
#9482=DIRECTION('ref_axis',(0.,0.,-1.));
#9483=DIRECTION('center_axis',(0.,1.,0.));
#9484=DIRECTION('ref_axis',(1.,0.,0.));
#9485=DIRECTION('center_axis',(0.,-1.,0.));
#9486=DIRECTION('ref_axis',(1.,0.,0.));
#9487=DIRECTION('center_axis',(0.,-1.,0.));
#9488=DIRECTION('ref_axis',(0.,0.,-1.));
#9489=DIRECTION('center_axis',(0.,0.,1.));
#9490=DIRECTION('ref_axis',(1.,0.,0.));
#9491=DIRECTION('center_axis',(0.,-1.,0.));
#9492=DIRECTION('ref_axis',(0.,0.,-1.));
#9493=DIRECTION('center_axis',(0.,1.,0.));
#9494=DIRECTION('ref_axis',(1.,0.,0.));
#9495=DIRECTION('center_axis',(0.,-1.,0.));
#9496=DIRECTION('ref_axis',(1.,0.,0.));
#9497=DIRECTION('center_axis',(0.,-1.,0.));
#9498=DIRECTION('ref_axis',(0.,0.,-1.));
#9499=DIRECTION('center_axis',(6.12323399573676E-17,0.,1.));
#9500=DIRECTION('ref_axis',(1.,0.,0.));
#9501=DIRECTION('center_axis',(0.,-1.,0.));
#9502=DIRECTION('ref_axis',(0.,0.,-1.));
#9503=DIRECTION('center_axis',(0.,1.,0.));
#9504=DIRECTION('ref_axis',(1.,0.,0.));
#9505=DIRECTION('center_axis',(0.,-1.,0.));
#9506=DIRECTION('ref_axis',(1.,0.,0.));
#9507=DIRECTION('center_axis',(0.,-1.,0.));
#9508=DIRECTION('ref_axis',(0.,0.,-1.));
#9509=DIRECTION('center_axis',(0.,0.,1.));
#9510=DIRECTION('ref_axis',(1.,0.,0.));
#9511=DIRECTION('center_axis',(0.,-1.,0.));
#9512=DIRECTION('ref_axis',(0.,0.,-1.));
#9513=DIRECTION('center_axis',(0.,1.,0.));
#9514=DIRECTION('ref_axis',(1.,0.,0.));
#9515=DIRECTION('center_axis',(0.,1.,0.));
#9516=DIRECTION('ref_axis',(1.,0.,0.));
#9517=DIRECTION('',(0.,1.,0.));
#9518=DIRECTION('center_axis',(0.,-1.,0.));
#9519=DIRECTION('ref_axis',(1.,0.,0.));
#9520=DIRECTION('center_axis',(0.,-1.,0.));
#9521=DIRECTION('ref_axis',(1.,0.,0.));
#9522=DIRECTION('center_axis',(0.,1.,0.));
#9523=DIRECTION('ref_axis',(1.,0.,0.));
#9524=DIRECTION('center_axis',(0.,-1.,0.));
#9525=DIRECTION('ref_axis',(0.,0.,-1.));
#9526=DIRECTION('center_axis',(0.,0.,1.));
#9527=DIRECTION('ref_axis',(1.,0.,0.));
#9528=DIRECTION('center_axis',(0.,-1.,0.));
#9529=DIRECTION('ref_axis',(0.,0.,-1.));
#9530=DIRECTION('center_axis',(0.,-1.,0.));
#9531=DIRECTION('ref_axis',(-1.,0.,0.));
#9532=DIRECTION('center_axis',(0.,1.,0.));
#9533=DIRECTION('ref_axis',(1.,0.,0.));
#9534=DIRECTION('axis',(0.,0.,1.));
#9535=DIRECTION('refdir',(1.,0.,0.));
#9536=DIRECTION('center_axis',(0.,1.,0.));
#9537=DIRECTION('ref_axis',(0.,0.,1.));
#9538=DIRECTION('center_axis',(0.,-1.,0.));
#9539=DIRECTION('ref_axis',(1.,0.,0.));
#9540=DIRECTION('center_axis',(0.,-1.,0.));
#9541=DIRECTION('ref_axis',(1.,0.,0.));
#9542=DIRECTION('center_axis',(0.,-1.,0.));
#9543=DIRECTION('ref_axis',(1.,0.,0.));
#9544=DIRECTION('center_axis',(0.,-1.,0.));
#9545=DIRECTION('ref_axis',(1.,0.,0.));
#9546=DIRECTION('',(0.,1.,0.));
#9547=DIRECTION('center_axis',(0.,-1.,0.));
#9548=DIRECTION('ref_axis',(0.,0.,-1.));
#9549=DIRECTION('center_axis',(0.,-1.,0.));
#9550=DIRECTION('ref_axis',(1.,0.,0.));
#9551=DIRECTION('center_axis',(0.,-1.,0.));
#9552=DIRECTION('ref_axis',(1.,0.,0.));
#9553=DIRECTION('',(0.,1.,0.));
#9554=DIRECTION('center_axis',(0.,1.,0.));
#9555=DIRECTION('ref_axis',(0.,0.,1.));
#9556=DIRECTION('center_axis',(0.,-1.,0.));
#9557=DIRECTION('ref_axis',(1.,0.,0.));
#9558=DIRECTION('center_axis',(0.,-1.,0.));
#9559=DIRECTION('ref_axis',(1.,0.,0.));
#9560=DIRECTION('center_axis',(0.,-1.,0.));
#9561=DIRECTION('ref_axis',(1.,0.,0.));
#9562=DIRECTION('center_axis',(0.,-1.,0.));
#9563=DIRECTION('ref_axis',(1.,0.,0.));
#9564=DIRECTION('',(0.,1.,0.));
#9565=DIRECTION('center_axis',(0.,-1.,0.));
#9566=DIRECTION('ref_axis',(0.,0.,-1.));
#9567=DIRECTION('center_axis',(0.,-1.,0.));
#9568=DIRECTION('ref_axis',(1.,0.,0.));
#9569=DIRECTION('center_axis',(0.,-1.,0.));
#9570=DIRECTION('ref_axis',(1.,0.,0.));
#9571=DIRECTION('',(0.,1.,0.));
#9572=DIRECTION('',(0.,0.,1.));
#9573=DIRECTION('',(1.,0.,0.));
#9574=DIRECTION('',(0.,0.,1.));
#9575=DIRECTION('',(1.,0.,0.));
#9576=DIRECTION('',(0.,0.,1.));
#9577=DIRECTION('',(1.,0.,0.));
#9578=DIRECTION('',(0.,0.,1.));
#9579=DIRECTION('',(1.,0.,0.));
#9580=DIRECTION('',(0.,0.,1.));
#9581=DIRECTION('',(1.,0.,0.));
#9582=DIRECTION('',(0.,0.,1.));
#9583=DIRECTION('',(1.,0.,0.));
#9584=DIRECTION('',(0.,0.,1.));
#9585=DIRECTION('',(1.,0.,0.));
#9586=DIRECTION('',(0.,0.,1.));
#9587=DIRECTION('',(1.,0.,0.));
#9588=DIRECTION('',(0.,0.,1.));
#9589=DIRECTION('',(1.,0.,0.));
#9590=DIRECTION('',(0.,0.,1.));
#9591=DIRECTION('',(1.,0.,0.));
#9592=DIRECTION('',(0.,0.,1.));
#9593=DIRECTION('',(1.,0.,0.));
#9594=DIRECTION('',(0.,0.,1.));
#9595=DIRECTION('',(1.,0.,0.));
#9596=DIRECTION('',(8.65956056235493E-17,-8.65956056235493E-17,-1.));
#9597=DIRECTION('',(2.22044604925031E-16,1.,-8.65956056235494E-17));
#9598=DIRECTION('',(8.65956056235493E-17,-8.65956056235493E-17,-1.));
#9599=DIRECTION('',(2.22044604925031E-16,1.,-8.65956056235494E-17));
#9600=DIRECTION('',(0.,-1.,2.22044604925031E-16));
#9601=DIRECTION('',(1.,0.,0.));
#9602=DIRECTION('',(0.,-1.,2.22044604925031E-16));
#9603=DIRECTION('',(1.,0.,0.));
#9604=DIRECTION('',(0.,-1.,2.22044604925031E-16));
#9605=DIRECTION('',(1.,0.,0.));
#9606=DIRECTION('',(0.,0.,1.));
#9607=DIRECTION('',(1.,0.,0.));
#9608=DIRECTION('axis',(0.,0.,1.));
#9609=DIRECTION('refdir',(1.,0.,0.));
#9610=DIRECTION('axis',(0.,0.,1.));
#9611=DIRECTION('refdir',(1.,0.,0.));
#9612=DIRECTION('center_axis',(0.,0.,1.));
#9613=DIRECTION('ref_axis',(1.,0.,0.));
#9614=DIRECTION('center_axis',(0.,0.,1.));
#9615=DIRECTION('ref_axis',(1.,0.,0.));
#9616=DIRECTION('',(0.,0.,1.));
#9617=DIRECTION('center_axis',(0.,0.,-1.));
#9618=DIRECTION('ref_axis',(1.,0.,0.));
#9619=DIRECTION('center_axis',(0.,1.,0.));
#9620=DIRECTION('ref_axis',(1.,0.,0.));
#9621=DIRECTION('center_axis',(0.,1.,0.));
#9622=DIRECTION('ref_axis',(1.,0.,0.));
#9623=DIRECTION('',(0.,1.,0.));
#9624=DIRECTION('center_axis',(0.,-1.,0.));
#9625=DIRECTION('ref_axis',(1.,0.,0.));
#9626=DIRECTION('center_axis',(0.,1.,0.));
#9627=DIRECTION('ref_axis',(1.,0.,0.));
#9628=DIRECTION('center_axis',(0.,1.,0.));
#9629=DIRECTION('ref_axis',(1.,0.,0.));
#9630=DIRECTION('',(0.,1.,0.));
#9631=DIRECTION('center_axis',(0.,-1.,0.));
#9632=DIRECTION('ref_axis',(1.,0.,0.));
#9633=DIRECTION('center_axis',(0.,0.,1.));
#9634=DIRECTION('ref_axis',(1.,0.,0.));
#9635=DIRECTION('',(-1.,0.,0.));
#9636=DIRECTION('',(0.,1.,0.));
#9637=DIRECTION('',(1.,0.,0.));
#9638=DIRECTION('',(0.,1.,0.));
#9639=DIRECTION('center_axis',(0.,0.,1.));
#9640=DIRECTION('ref_axis',(1.,0.,0.));
#9641=DIRECTION('',(-1.,0.,0.));
#9642=DIRECTION('',(0.,1.,0.));
#9643=DIRECTION('',(1.,0.,0.));
#9644=DIRECTION('',(0.,1.,0.));
#9645=DIRECTION('center_axis',(0.,1.,0.));
#9646=DIRECTION('ref_axis',(0.,0.,1.));
#9647=DIRECTION('',(0.,0.,-1.));
#9648=DIRECTION('',(-1.,0.,0.));
#9649=DIRECTION('',(0.,0.,1.));
#9650=DIRECTION('center_axis',(0.,1.,0.));
#9651=DIRECTION('ref_axis',(1.,0.,0.));
#9652=DIRECTION('',(0.,0.,1.));
#9653=DIRECTION('',(0.,0.,-1.));
#9654=DIRECTION('center_axis',(0.,1.,0.));
#9655=DIRECTION('ref_axis',(0.,0.,1.));
#9656=DIRECTION('',(0.,0.,1.));
#9657=DIRECTION('',(1.,0.,0.));
#9658=DIRECTION('',(0.,0.,-1.));
#9659=DIRECTION('center_axis',(-1.,0.,0.));
#9660=DIRECTION('ref_axis',(0.,0.,1.));
#9661=DIRECTION('',(0.,0.,-1.));
#9662=DIRECTION('',(0.,1.,0.));
#9663=DIRECTION('',(0.,1.,0.));
#9664=DIRECTION('center_axis',(0.,0.,-1.));
#9665=DIRECTION('ref_axis',(-1.,0.,0.));
#9666=DIRECTION('',(1.,0.,0.));
#9667=DIRECTION('',(0.,1.,0.));
#9668=DIRECTION('center_axis',(1.,0.,0.));
#9669=DIRECTION('ref_axis',(0.,0.,-1.));
#9670=DIRECTION('',(0.,0.,1.));
#9671=DIRECTION('',(0.,1.,0.));
#9672=DIRECTION('center_axis',(0.,0.,1.));
#9673=DIRECTION('ref_axis',(1.,0.,0.));
#9674=DIRECTION('',(-1.,0.,0.));
#9675=DIRECTION('center_axis',(0.,1.,0.));
#9676=DIRECTION('ref_axis',(1.,0.,0.));
#9677=DIRECTION('axis',(0.,0.,1.));
#9678=DIRECTION('refdir',(1.,0.,0.));
#9679=DIRECTION('center_axis',(0.,1.,0.));
#9680=DIRECTION('ref_axis',(1.,0.,0.));
#9681=DIRECTION('center_axis',(0.,1.,0.));
#9682=DIRECTION('ref_axis',(1.,0.,0.));
#9683=DIRECTION('',(0.,1.,0.));
#9684=DIRECTION('center_axis',(0.,-1.,0.));
#9685=DIRECTION('ref_axis',(1.,0.,0.));
#9686=DIRECTION('center_axis',(0.,1.,0.));
#9687=DIRECTION('ref_axis',(1.,0.,0.));
#9688=DIRECTION('center_axis',(0.,1.,0.));
#9689=DIRECTION('ref_axis',(1.,0.,0.));
#9690=DIRECTION('center_axis',(0.,1.,0.));
#9691=DIRECTION('ref_axis',(1.,0.,0.));
#9692=DIRECTION('',(0.,1.,0.));
#9693=DIRECTION('center_axis',(0.,1.,0.));
#9694=DIRECTION('ref_axis',(1.,0.,0.));
#9695=DIRECTION('center_axis',(0.,1.,0.));
#9696=DIRECTION('ref_axis',(1.,0.,0.));
#9697=DIRECTION('center_axis',(0.,1.,0.));
#9698=DIRECTION('ref_axis',(1.,0.,0.));
#9699=DIRECTION('center_axis',(0.,1.,0.));
#9700=DIRECTION('ref_axis',(1.,0.,0.));
#9701=DIRECTION('',(0.,-1.,0.));
#9702=DIRECTION('center_axis',(0.,1.,0.));
#9703=DIRECTION('ref_axis',(1.,0.,0.));
#9704=DIRECTION('center_axis',(0.,1.,0.));
#9705=DIRECTION('ref_axis',(1.,0.,0.));
#9706=DIRECTION('center_axis',(0.,1.,0.));
#9707=DIRECTION('ref_axis',(1.,0.,0.));
#9708=DIRECTION('axis',(0.,0.,1.));
#9709=DIRECTION('refdir',(1.,0.,0.));
#9710=DIRECTION('center_axis',(0.,1.,0.));
#9711=DIRECTION('ref_axis',(1.,0.,0.));
#9712=DIRECTION('center_axis',(0.,-1.,0.));
#9713=DIRECTION('ref_axis',(1.,0.,0.));
#9714=DIRECTION('',(0.,-1.,0.));
#9715=DIRECTION('center_axis',(0.,-1.,0.));
#9716=DIRECTION('ref_axis',(1.,0.,0.));
#9717=DIRECTION('center_axis',(0.,1.,0.));
#9718=DIRECTION('ref_axis',(1.,0.,0.));
#9719=DIRECTION('center_axis',(0.,1.,0.));
#9720=DIRECTION('ref_axis',(1.,0.,0.));
#9721=DIRECTION('',(0.,-1.,0.));
#9722=DIRECTION('center_axis',(0.,1.,0.));
#9723=DIRECTION('ref_axis',(1.,0.,0.));
#9724=DIRECTION('center_axis',(0.,1.,0.));
#9725=DIRECTION('ref_axis',(1.,0.,0.));
#9726=DIRECTION('center_axis',(0.,1.,0.));
#9727=DIRECTION('ref_axis',(1.,0.,0.));
#9728=DIRECTION('axis',(0.,0.,1.));
#9729=DIRECTION('refdir',(1.,0.,0.));
#9730=DIRECTION('center_axis',(0.,1.,0.));
#9731=DIRECTION('ref_axis',(1.,0.,0.));
#9732=DIRECTION('center_axis',(0.,-1.,0.));
#9733=DIRECTION('ref_axis',(1.,0.,0.));
#9734=DIRECTION('',(0.,-1.,0.));
#9735=DIRECTION('center_axis',(0.,-1.,0.));
#9736=DIRECTION('ref_axis',(1.,0.,0.));
#9737=DIRECTION('center_axis',(0.,1.,0.));
#9738=DIRECTION('ref_axis',(1.,0.,0.));
#9739=DIRECTION('center_axis',(0.,1.,0.));
#9740=DIRECTION('ref_axis',(1.,0.,0.));
#9741=DIRECTION('',(0.,-1.,0.));
#9742=DIRECTION('center_axis',(0.,1.,0.));
#9743=DIRECTION('ref_axis',(1.,0.,0.));
#9744=DIRECTION('center_axis',(0.,1.,0.));
#9745=DIRECTION('ref_axis',(1.,0.,0.));
#9746=DIRECTION('center_axis',(0.,1.,0.));
#9747=DIRECTION('ref_axis',(1.,0.,0.));
#9748=DIRECTION('axis',(0.,0.,1.));
#9749=DIRECTION('refdir',(1.,0.,0.));
#9750=DIRECTION('center_axis',(0.,1.,0.));
#9751=DIRECTION('ref_axis',(1.,0.,0.));
#9752=DIRECTION('center_axis',(0.,-1.,0.));
#9753=DIRECTION('ref_axis',(1.,0.,0.));
#9754=DIRECTION('',(0.,-1.,0.));
#9755=DIRECTION('center_axis',(0.,-1.,0.));
#9756=DIRECTION('ref_axis',(1.,0.,0.));
#9757=DIRECTION('center_axis',(0.,1.,0.));
#9758=DIRECTION('ref_axis',(1.,0.,0.));
#9759=DIRECTION('center_axis',(0.,1.,0.));
#9760=DIRECTION('ref_axis',(1.,0.,0.));
#9761=DIRECTION('',(0.,-1.,0.));
#9762=DIRECTION('center_axis',(0.,1.,0.));
#9763=DIRECTION('ref_axis',(1.,0.,0.));
#9764=DIRECTION('center_axis',(0.,1.,0.));
#9765=DIRECTION('ref_axis',(1.,0.,0.));
#9766=DIRECTION('center_axis',(0.,1.,0.));
#9767=DIRECTION('ref_axis',(1.,0.,0.));
#9768=DIRECTION('axis',(0.,0.,1.));
#9769=DIRECTION('refdir',(1.,0.,0.));
#9770=DIRECTION('center_axis',(0.,1.,0.));
#9771=DIRECTION('ref_axis',(1.,0.,0.));
#9772=DIRECTION('center_axis',(0.,-1.,0.));
#9773=DIRECTION('ref_axis',(1.,0.,0.));
#9774=DIRECTION('',(0.,-1.,0.));
#9775=DIRECTION('center_axis',(0.,-1.,0.));
#9776=DIRECTION('ref_axis',(1.,0.,0.));
#9777=DIRECTION('center_axis',(0.,1.,0.));
#9778=DIRECTION('ref_axis',(1.,0.,0.));
#9779=DIRECTION('center_axis',(0.,1.,0.));
#9780=DIRECTION('ref_axis',(1.,0.,0.));
#9781=DIRECTION('',(0.,-1.,0.));
#9782=DIRECTION('center_axis',(0.,1.,0.));
#9783=DIRECTION('ref_axis',(1.,0.,0.));
#9784=DIRECTION('center_axis',(0.,1.,0.));
#9785=DIRECTION('ref_axis',(1.,0.,0.));
#9786=DIRECTION('center_axis',(0.,1.,0.));
#9787=DIRECTION('ref_axis',(1.,0.,0.));
#9788=DIRECTION('axis',(0.,0.,1.));
#9789=DIRECTION('refdir',(1.,0.,0.));
#9790=DIRECTION('center_axis',(0.,1.,0.));
#9791=DIRECTION('ref_axis',(1.,0.,0.));
#9792=DIRECTION('center_axis',(0.,-1.,0.));
#9793=DIRECTION('ref_axis',(1.,0.,0.));
#9794=DIRECTION('',(0.,-1.,0.));
#9795=DIRECTION('center_axis',(0.,-1.,0.));
#9796=DIRECTION('ref_axis',(1.,0.,0.));
#9797=DIRECTION('center_axis',(0.,1.,0.));
#9798=DIRECTION('ref_axis',(1.,0.,0.));
#9799=DIRECTION('center_axis',(0.,1.,0.));
#9800=DIRECTION('ref_axis',(1.,0.,0.));
#9801=DIRECTION('',(0.,-1.,0.));
#9802=DIRECTION('center_axis',(0.,1.,0.));
#9803=DIRECTION('ref_axis',(1.,0.,0.));
#9804=DIRECTION('center_axis',(0.,1.,0.));
#9805=DIRECTION('ref_axis',(1.,0.,0.));
#9806=DIRECTION('center_axis',(0.,1.,0.));
#9807=DIRECTION('ref_axis',(1.,0.,0.));
#9808=DIRECTION('axis',(0.,0.,1.));
#9809=DIRECTION('refdir',(1.,0.,0.));
#9810=DIRECTION('center_axis',(0.,1.,0.));
#9811=DIRECTION('ref_axis',(1.,0.,0.));
#9812=DIRECTION('center_axis',(0.,-1.,0.));
#9813=DIRECTION('ref_axis',(1.,0.,0.));
#9814=DIRECTION('',(0.,-1.,0.));
#9815=DIRECTION('center_axis',(0.,-1.,0.));
#9816=DIRECTION('ref_axis',(1.,0.,0.));
#9817=DIRECTION('center_axis',(0.,1.,0.));
#9818=DIRECTION('ref_axis',(1.,0.,0.));
#9819=DIRECTION('center_axis',(0.,1.,0.));
#9820=DIRECTION('ref_axis',(1.,0.,0.));
#9821=DIRECTION('',(0.,-1.,0.));
#9822=DIRECTION('center_axis',(0.,1.,0.));
#9823=DIRECTION('ref_axis',(1.,0.,0.));
#9824=DIRECTION('center_axis',(0.,1.,0.));
#9825=DIRECTION('ref_axis',(1.,0.,0.));
#9826=DIRECTION('center_axis',(0.,1.,0.));
#9827=DIRECTION('ref_axis',(1.,0.,0.));
#9828=DIRECTION('axis',(0.,0.,1.));
#9829=DIRECTION('refdir',(1.,0.,0.));
#9830=DIRECTION('center_axis',(0.866025403784439,0.,-0.5));
#9831=DIRECTION('ref_axis',(0.5,0.,0.866025403784439));
#9832=DIRECTION('',(-0.5,0.,-0.866025403784439));
#9833=DIRECTION('',(0.,-1.,0.));
#9834=DIRECTION('',(0.5,0.,0.866025403784439));
#9835=DIRECTION('',(0.,-1.,0.));
#9836=DIRECTION('center_axis',(1.60246890531964E-16,0.,-1.));
#9837=DIRECTION('ref_axis',(1.,0.,1.60246890531964E-16));
#9838=DIRECTION('',(-1.,0.,-1.60246890531964E-16));
#9839=DIRECTION('',(0.,-1.,0.));
#9840=DIRECTION('',(1.,0.,1.60246890531964E-16));
#9841=DIRECTION('center_axis',(-0.866025403784439,0.,-0.5));
#9842=DIRECTION('ref_axis',(0.5,0.,-0.866025403784439));
#9843=DIRECTION('',(-0.5,0.,0.866025403784439));
#9844=DIRECTION('',(0.,-1.,0.));
#9845=DIRECTION('',(0.5,0.,-0.866025403784439));
#9846=DIRECTION('center_axis',(-0.866025403784439,0.,0.5));
#9847=DIRECTION('ref_axis',(-0.5,0.,-0.866025403784439));
#9848=DIRECTION('',(0.5,0.,0.866025403784439));
#9849=DIRECTION('',(0.,-1.,0.));
#9850=DIRECTION('',(-0.5,0.,-0.866025403784439));
#9851=DIRECTION('center_axis',(-1.60246890531964E-16,0.,1.));
#9852=DIRECTION('ref_axis',(-1.,0.,-1.60246890531964E-16));
#9853=DIRECTION('',(1.,0.,1.60246890531964E-16));
#9854=DIRECTION('',(0.,-1.,0.));
#9855=DIRECTION('',(-1.,0.,-1.60246890531964E-16));
#9856=DIRECTION('center_axis',(0.866025403784439,0.,0.5));
#9857=DIRECTION('ref_axis',(-0.5,0.,0.866025403784439));
#9858=DIRECTION('',(0.5,0.,-0.866025403784439));
#9859=DIRECTION('',(-0.5,0.,0.866025403784439));
#9860=DIRECTION('center_axis',(0.,1.,0.));
#9861=DIRECTION('ref_axis',(1.,0.,0.));
#9862=DIRECTION('center_axis',(0.,-1.,0.));
#9863=DIRECTION('ref_axis',(0.,0.,-1.));
#9864=DIRECTION('center_axis',(0.,1.,0.));
#9865=DIRECTION('ref_axis',(1.,0.,0.));
#9866=DIRECTION('center_axis',(0.,1.,0.));
#9867=DIRECTION('ref_axis',(1.,0.,0.));
#9868=DIRECTION('center_axis',(0.,1.,0.));
#9869=DIRECTION('ref_axis',(0.,0.,1.));
#9870=DIRECTION('center_axis',(0.,-1.,0.));
#9871=DIRECTION('ref_axis',(1.,0.,0.));
#9872=DIRECTION('center_axis',(0.,-1.,0.));
#9873=DIRECTION('ref_axis',(1.,0.,0.));
#9874=DIRECTION('center_axis',(0.,-1.,0.));
#9875=DIRECTION('ref_axis',(1.,0.,0.));
#9876=DIRECTION('',(0.707106781186547,0.707106781186548,8.65956056235493E-17));
#9877=DIRECTION('center_axis',(0.,-1.,0.));
#9878=DIRECTION('ref_axis',(1.,0.,0.));
#9879=DIRECTION('center_axis',(0.,-1.,0.));
#9880=DIRECTION('ref_axis',(1.,0.,0.));
#9881=DIRECTION('',(0.,1.,0.));
#9882=DIRECTION('center_axis',(0.,1.,0.));
#9883=DIRECTION('ref_axis',(1.,0.,0.));
#9884=DIRECTION('center_axis',(0.,-1.,0.));
#9885=DIRECTION('ref_axis',(1.,0.,0.));
#9886=DIRECTION('',(-0.707106781186547,0.707106781186548,-8.65956056235493E-17));
#9887=DIRECTION('center_axis',(0.,-1.,0.));
#9888=DIRECTION('ref_axis',(0.,0.,-1.));
#9889=DIRECTION('center_axis',(0.,-1.,0.));
#9890=DIRECTION('ref_axis',(1.,0.,0.));
#9891=DIRECTION('center_axis',(0.,1.,0.));
#9892=DIRECTION('ref_axis',(1.,0.,0.));
#9893=DIRECTION('center_axis',(0.,1.,0.));
#9894=DIRECTION('ref_axis',(1.,0.,0.));
#9895=DIRECTION('',(-0.447213595499958,0.894427190999916,-5.47678698264203E-17));
#9896=DIRECTION('center_axis',(0.,-1.,0.));
#9897=DIRECTION('ref_axis',(1.,0.,0.));
#9898=DIRECTION('',(0.,1.,0.));
#9899=DIRECTION('',(0.,0.,1.));
#9900=DIRECTION('',(1.,0.,0.));
#9901=DIRECTION('',(0.,0.,1.));
#9902=DIRECTION('',(1.,0.,0.));
#9903=DIRECTION('',(0.,0.,1.));
#9904=DIRECTION('',(1.,0.,0.));
#9905=DIRECTION('',(0.,0.,1.));
#9906=DIRECTION('',(1.,0.,0.));
#9907=DIRECTION('',(0.,0.,1.));
#9908=DIRECTION('',(1.,0.,0.));
#9909=DIRECTION('',(0.,0.,1.));
#9910=DIRECTION('',(1.,0.,0.));
#9911=DIRECTION('',(0.,0.,1.));
#9912=DIRECTION('',(1.,0.,0.));
#9913=DIRECTION('',(0.,0.,1.));
#9914=DIRECTION('',(1.,0.,0.));
#9915=DIRECTION('',(0.,0.,1.));
#9916=DIRECTION('',(-1.,1.22464679914735E-16,0.));
#9917=DIRECTION('',(0.,0.,1.));
#9918=DIRECTION('',(1.,0.,0.));
#9919=DIRECTION('',(0.,0.,1.));
#9920=DIRECTION('',(1.,0.,0.));
#9921=DIRECTION('',(0.,0.,1.));
#9922=DIRECTION('',(1.,0.,0.));
#9923=DIRECTION('',(0.,0.,1.));
#9924=DIRECTION('',(1.,0.,0.));
#9925=CARTESIAN_POINT('',(0.,0.,0.));
#9926=CARTESIAN_POINT('',(0.,0.,0.));
#9927=CARTESIAN_POINT('',(0.,0.,0.));
#9928=CARTESIAN_POINT('Origin',(4.4,1.,-0.1));
#9929=CARTESIAN_POINT('',(4.15,1.,0.));
#9930=CARTESIAN_POINT('Origin',(4.4,1.,0.));
#9931=CARTESIAN_POINT('',(4.15,1.,1.));
#9932=CARTESIAN_POINT('',(4.15,1.,-0.1));
#9933=CARTESIAN_POINT('Origin',(4.4,1.,1.));
#9934=CARTESIAN_POINT('Origin',(-4.4,5.,-0.1));
#9935=CARTESIAN_POINT('',(-4.65,5.,0.));
#9936=CARTESIAN_POINT('Origin',(-4.4,5.,0.));
#9937=CARTESIAN_POINT('',(-4.65,5.,1.));
#9938=CARTESIAN_POINT('',(-4.65,5.,-0.1));
#9939=CARTESIAN_POINT('Origin',(-4.4,5.,1.));
#9940=CARTESIAN_POINT('Origin',(-4.4,1.,-0.1));
#9941=CARTESIAN_POINT('',(-4.65,1.,0.));
#9942=CARTESIAN_POINT('Origin',(-4.4,1.,0.));
#9943=CARTESIAN_POINT('',(-4.65,1.,1.));
#9944=CARTESIAN_POINT('',(-4.65,1.,-0.1));
#9945=CARTESIAN_POINT('Origin',(-4.4,1.,1.));
#9946=CARTESIAN_POINT('Origin',(4.4,5.,-0.1));
#9947=CARTESIAN_POINT('',(4.15,5.,0.));
#9948=CARTESIAN_POINT('Origin',(4.4,5.,0.));
#9949=CARTESIAN_POINT('',(4.15,5.,1.));
#9950=CARTESIAN_POINT('',(4.15,5.,-0.1));
#9951=CARTESIAN_POINT('Origin',(4.4,5.,1.));
#9952=CARTESIAN_POINT('Origin',(11.,10.5,0.));
#9953=CARTESIAN_POINT('',(11.,10.5,0.));
#9954=CARTESIAN_POINT('',(-6.,10.5,0.));
#9955=CARTESIAN_POINT('',(11.,10.5,0.));
#9956=CARTESIAN_POINT('',(-6.,10.5,1.));
#9957=CARTESIAN_POINT('',(-6.,10.5,0.));
#9958=CARTESIAN_POINT('',(11.,10.5,1.));
#9959=CARTESIAN_POINT('',(11.,10.5,1.));
#9960=CARTESIAN_POINT('',(11.,10.5,0.));
#9961=CARTESIAN_POINT('Origin',(11.,-2.,0.));
#9962=CARTESIAN_POINT('',(11.,-2.,0.));
#9963=CARTESIAN_POINT('',(11.,-2.,0.));
#9964=CARTESIAN_POINT('',(11.,-2.,1.));
#9965=CARTESIAN_POINT('',(11.,-2.,1.));
#9966=CARTESIAN_POINT('',(11.,-2.,0.));
#9967=CARTESIAN_POINT('Origin',(-6.,-2.,0.));
#9968=CARTESIAN_POINT('',(-6.,-2.,0.));
#9969=CARTESIAN_POINT('',(-6.,-2.,0.));
#9970=CARTESIAN_POINT('',(-6.,-2.,1.));
#9971=CARTESIAN_POINT('',(-6.,-2.,1.));
#9972=CARTESIAN_POINT('',(-6.,-2.,0.));
#9973=CARTESIAN_POINT('Origin',(-6.,10.5,0.));
#9974=CARTESIAN_POINT('',(-6.,10.5,0.));
#9975=CARTESIAN_POINT('',(-6.,10.5,1.));
#9976=CARTESIAN_POINT('Origin',(2.5,4.25,1.));
#9977=CARTESIAN_POINT('Origin',(2.5,4.25,0.));
#9978=CARTESIAN_POINT('',(0.,0.,0.));
#9979=CARTESIAN_POINT('Origin',(-3.3,4.4,8.));
#9980=CARTESIAN_POINT('',(-3.465,4.4,8.));
#9981=CARTESIAN_POINT('Origin',(-3.3,4.4,8.));
#9982=CARTESIAN_POINT('',(-3.465,6.,8.));
#9983=CARTESIAN_POINT('',(-3.465,4.4,8.));
#9984=CARTESIAN_POINT('Origin',(-3.3,6.,8.));
#9985=CARTESIAN_POINT('Origin',(-3.3,4.4,8.));
#9986=CARTESIAN_POINT('Origin',(2.02066721859313E-16,4.4,11.3));
#9987=CARTESIAN_POINT('',(-0.165,4.4,11.3));
#9988=CARTESIAN_POINT('Origin',(2.02066721859313E-16,4.4,11.3));
#9989=CARTESIAN_POINT('',(-0.165,6.,11.3));
#9990=CARTESIAN_POINT('',(-0.165,4.4,11.3));
#9991=CARTESIAN_POINT('Origin',(2.02066721859313E-16,6.,11.3));
#9992=CARTESIAN_POINT('Origin',(1.94289029309402E-16,4.4,11.3));
#9993=CARTESIAN_POINT('Origin',(3.3,4.4,8.));
#9994=CARTESIAN_POINT('',(3.135,4.4,8.));
#9995=CARTESIAN_POINT('Origin',(3.3,4.4,8.));
#9996=CARTESIAN_POINT('',(3.135,6.,8.));
#9997=CARTESIAN_POINT('',(3.135,4.4,8.));
#9998=CARTESIAN_POINT('Origin',(3.3,6.,8.));
#9999=CARTESIAN_POINT('Origin',(3.3,4.4,8.));
#10000=CARTESIAN_POINT('Origin',(-6.0620016557794E-16,4.4,4.7));
#10001=CARTESIAN_POINT('',(-0.165000000000001,4.4,4.7));
#10002=CARTESIAN_POINT('Origin',(-6.0620016557794E-16,4.4,4.7));
#10003=CARTESIAN_POINT('',(-0.165000000000001,6.,4.7));
#10004=CARTESIAN_POINT('',(-0.165000000000001,4.4,4.7));
#10005=CARTESIAN_POINT('Origin',(-6.0620016557794E-16,6.,4.7));
#10006=CARTESIAN_POINT('Origin',(-6.10622663543836E-16,4.4,4.7));
#10007=CARTESIAN_POINT('Origin',(-3.3,-0.1,8.));
#10008=CARTESIAN_POINT('',(-3.465,0.,8.));
#10009=CARTESIAN_POINT('Origin',(-3.3,0.,8.));
#10010=CARTESIAN_POINT('',(-3.465,1.6,8.));
#10011=CARTESIAN_POINT('',(-3.465,-0.1,8.));
#10012=CARTESIAN_POINT('Origin',(-3.3,1.6,8.));
#10013=CARTESIAN_POINT('Origin',(-3.3,1.6,8.));
#10014=CARTESIAN_POINT('Origin',(2.02066721859313E-16,-0.1,11.3));
#10015=CARTESIAN_POINT('',(-0.165,0.,11.3));
#10016=CARTESIAN_POINT('Origin',(2.02066721859313E-16,0.,11.3));
#10017=CARTESIAN_POINT('',(-0.165,1.6,11.3));
#10018=CARTESIAN_POINT('',(-0.165,-0.1,11.3));
#10019=CARTESIAN_POINT('Origin',(2.02066721859313E-16,1.6,11.3));
#10020=CARTESIAN_POINT('Origin',(1.94289029309402E-16,1.6,11.3));
#10021=CARTESIAN_POINT('Origin',(3.3,-0.1,8.));
#10022=CARTESIAN_POINT('',(3.135,0.,8.));
#10023=CARTESIAN_POINT('Origin',(3.3,0.,8.));
#10024=CARTESIAN_POINT('',(3.135,1.6,8.));
#10025=CARTESIAN_POINT('',(3.135,-0.1,8.));
#10026=CARTESIAN_POINT('Origin',(3.3,1.6,8.));
#10027=CARTESIAN_POINT('Origin',(3.3,1.6,8.));
#10028=CARTESIAN_POINT('Origin',(-6.0620016557794E-16,-0.1,4.7));
#10029=CARTESIAN_POINT('',(-0.165000000000001,0.,4.7));
#10030=CARTESIAN_POINT('Origin',(-6.0620016557794E-16,0.,4.7));
#10031=CARTESIAN_POINT('',(-0.165000000000001,1.6,4.7));
#10032=CARTESIAN_POINT('',(-0.165000000000001,-0.1,4.7));
#10033=CARTESIAN_POINT('Origin',(-6.0620016557794E-16,1.6,4.7));
#10034=CARTESIAN_POINT('Origin',(-6.10622663543836E-16,1.6,4.7));
#10035=CARTESIAN_POINT('Origin',(4.4,1.,2.5));
#10036=CARTESIAN_POINT('',(4.73166247903554,0.5,4.8));
#10037=CARTESIAN_POINT('',(4.73166247903554,0.5,2.5));
#10038=CARTESIAN_POINT('',(4.73166247903554,0.5,2.5));
#10039=CARTESIAN_POINT('',(4.73166247903554,1.5,4.8));
#10040=CARTESIAN_POINT('Origin',(4.4,1.,4.8));
#10041=CARTESIAN_POINT('',(4.73166247903554,1.5,2.5));
#10042=CARTESIAN_POINT('',(4.73166247903554,1.5,2.5));
#10043=CARTESIAN_POINT('Origin',(4.4,1.,2.5));
#10044=CARTESIAN_POINT('Origin',(4.4,1.,2.5));
#10045=CARTESIAN_POINT('',(4.06833752096446,0.5,2.5));
#10046=CARTESIAN_POINT('',(4.06833752096446,0.5,4.8));
#10047=CARTESIAN_POINT('',(4.06833752096446,0.5,2.5));
#10048=CARTESIAN_POINT('',(4.06833752096446,1.5,2.5));
#10049=CARTESIAN_POINT('Origin',(4.4,1.,2.5));
#10050=CARTESIAN_POINT('',(4.06833752096446,1.5,4.8));
#10051=CARTESIAN_POINT('',(4.06833752096446,1.5,2.5));
#10052=CARTESIAN_POINT('Origin',(4.4,1.,4.8));
#10053=CARTESIAN_POINT('Origin',(4.4,1.,2.5));
#10054=CARTESIAN_POINT('',(2.2,0.5,2.5));
#10055=CARTESIAN_POINT('',(2.2,1.5,2.5));
#10056=CARTESIAN_POINT('',(4.07,1.,2.5));
#10057=CARTESIAN_POINT('Origin',(4.4,1.,2.5));
#10058=CARTESIAN_POINT('Origin',(-4.4,5.,2.5));
#10059=CARTESIAN_POINT('',(-4.06833752096446,4.5,4.8));
#10060=CARTESIAN_POINT('',(-4.06833752096446,4.5,2.5));
#10061=CARTESIAN_POINT('',(-4.06833752096446,4.5,2.5));
#10062=CARTESIAN_POINT('',(-4.06833752096446,5.5,4.8));
#10063=CARTESIAN_POINT('Origin',(-4.4,5.,4.8));
#10064=CARTESIAN_POINT('',(-4.06833752096446,5.5,2.5));
#10065=CARTESIAN_POINT('',(-4.06833752096446,5.5,2.5));
#10066=CARTESIAN_POINT('Origin',(-4.4,5.,2.5));
#10067=CARTESIAN_POINT('Origin',(-4.4,5.,2.5));
#10068=CARTESIAN_POINT('',(-4.73166247903554,4.5,2.5));
#10069=CARTESIAN_POINT('',(-4.73166247903554,4.5,4.8));
#10070=CARTESIAN_POINT('',(-4.73166247903554,4.5,2.5));
#10071=CARTESIAN_POINT('',(-4.73166247903554,5.5,2.5));
#10072=CARTESIAN_POINT('Origin',(-4.4,5.,2.5));
#10073=CARTESIAN_POINT('',(-4.73166247903554,5.5,4.8));
#10074=CARTESIAN_POINT('',(-4.73166247903554,5.5,2.5));
#10075=CARTESIAN_POINT('Origin',(-4.4,5.,4.8));
#10076=CARTESIAN_POINT('Origin',(-4.4,5.,2.5));
#10077=CARTESIAN_POINT('',(-2.2,4.5,2.5));
#10078=CARTESIAN_POINT('',(-2.2,5.5,2.5));
#10079=CARTESIAN_POINT('',(-4.73,5.,2.5));
#10080=CARTESIAN_POINT('Origin',(-4.4,5.,2.5));
#10081=CARTESIAN_POINT('Origin',(-4.4,1.,2.5));
#10082=CARTESIAN_POINT('',(-4.06833752096446,0.5,4.8));
#10083=CARTESIAN_POINT('',(-4.06833752096446,0.5,2.5));
#10084=CARTESIAN_POINT('',(-4.06833752096446,0.5,2.5));
#10085=CARTESIAN_POINT('',(-4.06833752096446,1.5,4.8));
#10086=CARTESIAN_POINT('Origin',(-4.4,1.,4.8));
#10087=CARTESIAN_POINT('',(-4.06833752096446,1.5,2.5));
#10088=CARTESIAN_POINT('',(-4.06833752096446,1.5,2.5));
#10089=CARTESIAN_POINT('Origin',(-4.4,1.,2.5));
#10090=CARTESIAN_POINT('Origin',(-4.4,1.,2.5));
#10091=CARTESIAN_POINT('',(-4.73166247903554,0.5,2.5));
#10092=CARTESIAN_POINT('',(-4.73166247903554,0.5,4.8));
#10093=CARTESIAN_POINT('',(-4.73166247903554,0.5,2.5));
#10094=CARTESIAN_POINT('',(-4.73166247903554,1.5,2.5));
#10095=CARTESIAN_POINT('Origin',(-4.4,1.,2.5));
#10096=CARTESIAN_POINT('',(-4.73166247903554,1.5,4.8));
#10097=CARTESIAN_POINT('',(-4.73166247903554,1.5,2.5));
#10098=CARTESIAN_POINT('Origin',(-4.4,1.,4.8));
#10099=CARTESIAN_POINT('Origin',(-4.4,1.,2.5));
#10100=CARTESIAN_POINT('',(-2.2,0.5,2.5));
#10101=CARTESIAN_POINT('',(-2.2,1.5,2.5));
#10102=CARTESIAN_POINT('',(-4.73,1.,2.5));
#10103=CARTESIAN_POINT('Origin',(-4.4,1.,2.5));
#10104=CARTESIAN_POINT('Origin',(4.4,5.,2.5));
#10105=CARTESIAN_POINT('',(4.73166247903554,4.5,4.8));
#10106=CARTESIAN_POINT('',(4.73166247903554,4.5,2.5));
#10107=CARTESIAN_POINT('',(4.73166247903554,4.5,2.5));
#10108=CARTESIAN_POINT('',(4.73166247903554,5.5,4.8));
#10109=CARTESIAN_POINT('Origin',(4.4,5.,4.8));
#10110=CARTESIAN_POINT('',(4.73166247903554,5.5,2.5));
#10111=CARTESIAN_POINT('',(4.73166247903554,5.5,2.5));
#10112=CARTESIAN_POINT('Origin',(4.4,5.,2.5));
#10113=CARTESIAN_POINT('Origin',(4.4,5.,2.5));
#10114=CARTESIAN_POINT('',(4.06833752096446,4.5,2.5));
#10115=CARTESIAN_POINT('',(4.06833752096446,4.5,4.8));
#10116=CARTESIAN_POINT('',(4.06833752096446,4.5,2.5));
#10117=CARTESIAN_POINT('',(4.06833752096446,5.5,2.5));
#10118=CARTESIAN_POINT('Origin',(4.4,5.,2.5));
#10119=CARTESIAN_POINT('',(4.06833752096446,5.5,4.8));
#10120=CARTESIAN_POINT('',(4.06833752096446,5.5,2.5));
#10121=CARTESIAN_POINT('Origin',(4.4,5.,4.8));
#10122=CARTESIAN_POINT('Origin',(4.4,5.,2.5));
#10123=CARTESIAN_POINT('',(2.2,4.5,2.5));
#10124=CARTESIAN_POINT('',(2.2,5.5,2.5));
#10125=CARTESIAN_POINT('',(4.07,5.,2.5));
#10126=CARTESIAN_POINT('Origin',(4.4,5.,2.5));
#10127=CARTESIAN_POINT('Origin',(-5.2,0.5,4.8));
#10128=CARTESIAN_POINT('',(5.2,0.5,4.8));
#10129=CARTESIAN_POINT('',(5.2,0.5,4.8));
#10130=CARTESIAN_POINT('',(5.2,1.5,4.8));
#10131=CARTESIAN_POINT('',(5.2,0.5,4.8));
#10132=CARTESIAN_POINT('',(5.2,1.5,4.8));
#10133=CARTESIAN_POINT('Origin',(-5.2,0.5,4.8));
#10134=CARTESIAN_POINT('',(2.4,1.5,4.8));
#10135=CARTESIAN_POINT('',(5.2,1.5,4.8));
#10136=CARTESIAN_POINT('',(2.4,0.5,4.8));
#10137=CARTESIAN_POINT('',(2.4,0.,4.8));
#10138=CARTESIAN_POINT('',(5.2,0.5,4.8));
#10139=CARTESIAN_POINT('Origin',(-5.2,4.5,4.8));
#10140=CARTESIAN_POINT('',(-2.4,4.5,4.8));
#10141=CARTESIAN_POINT('',(5.2,4.5,4.8));
#10142=CARTESIAN_POINT('',(-2.4,5.5,4.8));
#10143=CARTESIAN_POINT('',(-2.4,0.,4.8));
#10144=CARTESIAN_POINT('',(5.2,5.5,4.8));
#10145=CARTESIAN_POINT('Origin',(-5.2,4.5,4.8));
#10146=CARTESIAN_POINT('',(-5.2,5.5,4.8));
#10147=CARTESIAN_POINT('',(5.2,5.5,4.8));
#10148=CARTESIAN_POINT('',(-5.2,4.5,4.8));
#10149=CARTESIAN_POINT('',(-5.2,4.5,4.8));
#10150=CARTESIAN_POINT('',(5.2,4.5,4.8));
#10151=CARTESIAN_POINT('Origin',(0.,1.5,2.9));
#10152=CARTESIAN_POINT('',(5.2,1.5,1.));
#10153=CARTESIAN_POINT('',(5.2,1.5,1.));
#10154=CARTESIAN_POINT('',(-5.2,1.5,1.));
#10155=CARTESIAN_POINT('',(-5.2,1.5,1.));
#10156=CARTESIAN_POINT('',(-5.2,1.5,4.8));
#10157=CARTESIAN_POINT('',(-5.2,1.5,4.8));
#10158=CARTESIAN_POINT('',(5.2,1.5,4.8));
#10159=CARTESIAN_POINT('',(-2.4,1.5,4.8));
#10160=CARTESIAN_POINT('',(5.2,1.5,4.8));
#10161=CARTESIAN_POINT('Origin',(0.,1.5,8.));
#10162=CARTESIAN_POINT('Origin',(-5.2,0.5,4.8));
#10163=CARTESIAN_POINT('',(-2.4,0.5,4.8));
#10164=CARTESIAN_POINT('',(5.2,0.5,4.8));
#10165=CARTESIAN_POINT('',(-2.4,0.,4.8));
#10166=CARTESIAN_POINT('Origin',(-5.2,0.5,4.8));
#10167=CARTESIAN_POINT('',(-5.2,0.5,4.8));
#10168=CARTESIAN_POINT('',(-5.2,0.5,4.8));
#10169=CARTESIAN_POINT('',(5.2,0.5,4.8));
#10170=CARTESIAN_POINT('Origin',(0.,5.5,2.9));
#10171=CARTESIAN_POINT('',(2.4,5.5,4.8));
#10172=CARTESIAN_POINT('Origin',(0.,5.5,8.));
#10173=CARTESIAN_POINT('',(5.2,5.5,4.8));
#10174=CARTESIAN_POINT('',(5.2,5.5,4.8));
#10175=CARTESIAN_POINT('',(5.2,5.5,4.8));
#10176=CARTESIAN_POINT('',(5.2,5.5,1.));
#10177=CARTESIAN_POINT('',(5.2,5.5,1.));
#10178=CARTESIAN_POINT('',(-5.2,5.5,1.));
#10179=CARTESIAN_POINT('',(-5.2,5.5,1.));
#10180=CARTESIAN_POINT('',(-5.2,5.5,4.8));
#10181=CARTESIAN_POINT('Origin',(-5.2,4.5,4.8));
#10182=CARTESIAN_POINT('',(5.2,4.5,4.8));
#10183=CARTESIAN_POINT('',(5.2,4.5,4.8));
#10184=CARTESIAN_POINT('',(5.2,4.5,4.8));
#10185=CARTESIAN_POINT('Origin',(-5.2,4.5,4.8));
#10186=CARTESIAN_POINT('',(2.4,4.5,4.8));
#10187=CARTESIAN_POINT('',(2.4,0.,4.8));
#10188=CARTESIAN_POINT('',(5.2,4.5,4.8));
#10189=CARTESIAN_POINT('Origin',(4.4,1.,0.9));
#10190=CARTESIAN_POINT('',(4.07,1.,1.));
#10191=CARTESIAN_POINT('Origin',(4.4,1.,1.));
#10192=CARTESIAN_POINT('',(4.07,1.,0.9));
#10193=CARTESIAN_POINT('Origin',(-4.4,5.,0.9));
#10194=CARTESIAN_POINT('',(-4.73,5.,1.));
#10195=CARTESIAN_POINT('Origin',(-4.4,5.,1.));
#10196=CARTESIAN_POINT('',(-4.73,5.,0.9));
#10197=CARTESIAN_POINT('Origin',(-4.4,1.,0.9));
#10198=CARTESIAN_POINT('',(-4.73,1.,1.));
#10199=CARTESIAN_POINT('Origin',(-4.4,1.,1.));
#10200=CARTESIAN_POINT('',(-4.73,1.,0.9));
#10201=CARTESIAN_POINT('Origin',(4.4,5.,0.9));
#10202=CARTESIAN_POINT('',(4.07,5.,1.));
#10203=CARTESIAN_POINT('Origin',(4.4,5.,1.));
#10204=CARTESIAN_POINT('',(4.07,5.,0.9));
#10205=CARTESIAN_POINT('Origin',(-5.2,4.5,1.));
#10206=CARTESIAN_POINT('',(-5.2,4.5,1.));
#10207=CARTESIAN_POINT('',(-5.2,4.5,4.8));
#10208=CARTESIAN_POINT('',(-5.2,4.5,1.));
#10209=CARTESIAN_POINT('Origin',(5.2,4.5,1.));
#10210=CARTESIAN_POINT('',(5.2,4.5,1.));
#10211=CARTESIAN_POINT('',(-5.2,4.5,1.));
#10212=CARTESIAN_POINT('',(5.2,4.5,1.));
#10213=CARTESIAN_POINT('Origin',(5.2,4.5,4.8));
#10214=CARTESIAN_POINT('',(5.2,4.5,1.));
#10215=CARTESIAN_POINT('Origin',(0.,4.5,2.9));
#10216=CARTESIAN_POINT('Origin',(0.,4.5,8.));
#10217=CARTESIAN_POINT('Origin',(-5.2,0.5,1.));
#10218=CARTESIAN_POINT('',(-5.2,0.5,1.));
#10219=CARTESIAN_POINT('',(-5.2,0.5,4.8));
#10220=CARTESIAN_POINT('',(-5.2,0.5,1.));
#10221=CARTESIAN_POINT('Origin',(5.2,0.5,1.));
#10222=CARTESIAN_POINT('',(5.2,0.5,1.));
#10223=CARTESIAN_POINT('',(-5.2,0.5,1.));
#10224=CARTESIAN_POINT('',(5.2,0.5,1.));
#10225=CARTESIAN_POINT('Origin',(5.2,0.5,4.8));
#10226=CARTESIAN_POINT('',(5.2,0.5,1.));
#10227=CARTESIAN_POINT('Origin',(0.,0.5,2.9));
#10228=CARTESIAN_POINT('Origin',(0.,0.5,8.));
#10229=CARTESIAN_POINT('Origin',(0.,0.,8.));
#10230=CARTESIAN_POINT('',(-2.6,6.,8.));
#10231=CARTESIAN_POINT('Origin',(0.,6.,8.));
#10232=CARTESIAN_POINT('',(-2.6,0.,8.));
#10233=CARTESIAN_POINT('',(-2.6,0.,8.));
#10234=CARTESIAN_POINT('Origin',(0.,0.,8.));
#10235=CARTESIAN_POINT('Origin',(0.,0.,8.));
#10236=CARTESIAN_POINT('',(-4.,6.,8.));
#10237=CARTESIAN_POINT('Origin',(0.,6.,8.));
#10238=CARTESIAN_POINT('',(-4.,0.,8.));
#10239=CARTESIAN_POINT('',(-4.,0.,8.));
#10240=CARTESIAN_POINT('Origin',(0.,0.,8.));
#10241=CARTESIAN_POINT('Origin',(0.,6.,8.));
#10242=CARTESIAN_POINT('Origin',(0.,0.,8.));
#10243=CARTESIAN_POINT('',(0.,0.,0.));
#10244=CARTESIAN_POINT('Origin',(0.,1.75,8.));
#10245=CARTESIAN_POINT('',(-2.,4.25,8.));
#10246=CARTESIAN_POINT('Origin',(0.,4.25,8.));
#10247=CARTESIAN_POINT('',(-2.,1.75,8.));
#10248=CARTESIAN_POINT('',(-2.,1.75,8.));
#10249=CARTESIAN_POINT('Origin',(0.,1.75,8.));
#10250=CARTESIAN_POINT('Origin',(0.,1.75,8.));
#10251=CARTESIAN_POINT('',(-2.59,4.25,8.));
#10252=CARTESIAN_POINT('Origin',(0.,4.25,8.));
#10253=CARTESIAN_POINT('',(-2.59,1.75,8.));
#10254=CARTESIAN_POINT('',(-2.59,1.75,8.));
#10255=CARTESIAN_POINT('Origin',(0.,1.75,8.));
#10256=CARTESIAN_POINT('Origin',(0.,4.25,8.));
#10257=CARTESIAN_POINT('Origin',(0.,1.75,8.));
#10258=CARTESIAN_POINT('',(0.,0.,0.));
#10259=CARTESIAN_POINT('Origin',(-3.3,-0.5,8.));
#10260=CARTESIAN_POINT('',(-3.525,-0.4,8.));
#10261=CARTESIAN_POINT('Origin',(-3.3,-0.4,8.));
#10262=CARTESIAN_POINT('',(-3.525,0.,8.));
#10263=CARTESIAN_POINT('',(-3.525,-0.5,8.));
#10264=CARTESIAN_POINT('Origin',(-3.3,0.,8.));
#10265=CARTESIAN_POINT('Origin',(2.02066721859313E-16,-0.5,11.3));
#10266=CARTESIAN_POINT('',(-0.225,-0.4,11.3));
#10267=CARTESIAN_POINT('Origin',(2.02066721859313E-16,-0.4,11.3));
#10268=CARTESIAN_POINT('',(-0.225,0.,11.3));
#10269=CARTESIAN_POINT('',(-0.225,-0.5,11.3));
#10270=CARTESIAN_POINT('Origin',(2.02066721859313E-16,0.,11.3));
#10271=CARTESIAN_POINT('Origin',(3.3,-0.5,8.));
#10272=CARTESIAN_POINT('',(3.075,-0.4,8.));
#10273=CARTESIAN_POINT('Origin',(3.3,-0.4,8.));
#10274=CARTESIAN_POINT('',(3.075,0.,8.));
#10275=CARTESIAN_POINT('',(3.075,-0.5,8.));
#10276=CARTESIAN_POINT('Origin',(3.3,0.,8.));
#10277=CARTESIAN_POINT('Origin',(-6.0620016557794E-16,-0.5,4.7));
#10278=CARTESIAN_POINT('',(-0.225000000000001,-0.4,4.7));
#10279=CARTESIAN_POINT('Origin',(-6.0620016557794E-16,-0.4,4.7));
#10280=CARTESIAN_POINT('',(-0.225000000000001,0.,4.7));
#10281=CARTESIAN_POINT('',(-0.225000000000001,-0.5,4.7));
#10282=CARTESIAN_POINT('Origin',(-6.0620016557794E-16,0.,4.7));
#10283=CARTESIAN_POINT('Origin',(0.,0.,8.));
#10284=CARTESIAN_POINT('',(-2.59,0.25,8.));
#10285=CARTESIAN_POINT('Origin',(0.,0.25,8.));
#10286=CARTESIAN_POINT('',(-2.59,0.,8.));
#10287=CARTESIAN_POINT('',(-2.59,0.,8.));
#10288=CARTESIAN_POINT('Origin',(0.,0.,8.));
#10289=CARTESIAN_POINT('Origin',(0.,0.25,8.));
#10290=CARTESIAN_POINT('',(-2.,0.25,8.));
#10291=CARTESIAN_POINT('Origin',(0.,0.25,8.));
#10292=CARTESIAN_POINT('Origin',(0.,-0.4,8.));
#10293=CARTESIAN_POINT('',(-2.,-0.4,8.));
#10294=CARTESIAN_POINT('',(-2.,-0.4,8.));
#10295=CARTESIAN_POINT('Origin',(0.,-0.4,8.));
#10296=CARTESIAN_POINT('Origin',(0.,-0.4,8.));
#10297=CARTESIAN_POINT('',(-4.,0.,8.));
#10298=CARTESIAN_POINT('Origin',(0.,0.,8.));
#10299=CARTESIAN_POINT('',(-4.,-0.4,8.));
#10300=CARTESIAN_POINT('',(-4.,-0.4,8.));
#10301=CARTESIAN_POINT('Origin',(0.,-0.4,8.));
#10302=CARTESIAN_POINT('Origin',(0.,0.,8.));
#10303=CARTESIAN_POINT('Origin',(0.,-0.4,8.));
#10304=CARTESIAN_POINT('',(0.,0.,0.));
#10305=CARTESIAN_POINT('Origin',(-3.3,5.9,8.));
#10306=CARTESIAN_POINT('',(-3.525,6.,8.));
#10307=CARTESIAN_POINT('Origin',(-3.3,6.,8.));
#10308=CARTESIAN_POINT('',(-3.525,6.4,8.));
#10309=CARTESIAN_POINT('',(-3.525,5.9,8.));
#10310=CARTESIAN_POINT('Origin',(-3.3,6.4,8.));
#10311=CARTESIAN_POINT('Origin',(2.02066721859313E-16,5.9,11.3));
#10312=CARTESIAN_POINT('',(-0.225,6.,11.3));
#10313=CARTESIAN_POINT('Origin',(2.02066721859313E-16,6.,11.3));
#10314=CARTESIAN_POINT('',(-0.225,6.4,11.3));
#10315=CARTESIAN_POINT('',(-0.225,5.9,11.3));
#10316=CARTESIAN_POINT('Origin',(2.02066721859313E-16,6.4,11.3));
#10317=CARTESIAN_POINT('Origin',(3.3,5.9,8.));
#10318=CARTESIAN_POINT('',(3.075,6.,8.));
#10319=CARTESIAN_POINT('Origin',(3.3,6.,8.));
#10320=CARTESIAN_POINT('',(3.075,6.4,8.));
#10321=CARTESIAN_POINT('',(3.075,5.9,8.));
#10322=CARTESIAN_POINT('Origin',(3.3,6.4,8.));
#10323=CARTESIAN_POINT('Origin',(-6.0620016557794E-16,5.9,4.7));
#10324=CARTESIAN_POINT('',(-0.225000000000001,6.,4.7));
#10325=CARTESIAN_POINT('Origin',(-6.0620016557794E-16,6.,4.7));
#10326=CARTESIAN_POINT('',(-0.225000000000001,6.4,4.7));
#10327=CARTESIAN_POINT('',(-0.225000000000001,5.9,4.7));
#10328=CARTESIAN_POINT('Origin',(-6.0620016557794E-16,6.4,4.7));
#10329=CARTESIAN_POINT('Origin',(0.,5.75,8.));
#10330=CARTESIAN_POINT('',(-2.59,6.,8.));
#10331=CARTESIAN_POINT('Origin',(0.,6.,8.));
#10332=CARTESIAN_POINT('',(-2.59,5.75,8.));
#10333=CARTESIAN_POINT('',(-2.59,5.75,8.));
#10334=CARTESIAN_POINT('Origin',(0.,5.75,8.));
#10335=CARTESIAN_POINT('Origin',(0.,5.75,8.));
#10336=CARTESIAN_POINT('',(-2.,5.75,8.));
#10337=CARTESIAN_POINT('Origin',(0.,5.75,8.));
#10338=CARTESIAN_POINT('Origin',(0.,6.,8.));
#10339=CARTESIAN_POINT('',(-2.,6.4,8.));
#10340=CARTESIAN_POINT('Origin',(0.,6.4,8.));
#10341=CARTESIAN_POINT('',(-2.,6.,8.));
#10342=CARTESIAN_POINT('Origin',(0.,6.,8.));
#10343=CARTESIAN_POINT('',(-4.,6.4,8.));
#10344=CARTESIAN_POINT('Origin',(0.,6.4,8.));
#10345=CARTESIAN_POINT('',(-4.,6.,8.));
#10346=CARTESIAN_POINT('',(-4.,6.,8.));
#10347=CARTESIAN_POINT('Origin',(0.,6.,8.));
#10348=CARTESIAN_POINT('Origin',(0.,6.4,8.));
#10349=CARTESIAN_POINT('Origin',(0.,6.,8.));
#10350=CARTESIAN_POINT('',(0.,0.,0.));
#10351=CARTESIAN_POINT('Origin',(-4.,10.5,-0.8));
#10352=CARTESIAN_POINT('',(-4.,10.5,-0.8));
#10353=CARTESIAN_POINT('',(-6.,10.5,-0.8));
#10354=CARTESIAN_POINT('',(-4.,10.5,-0.8));
#10355=CARTESIAN_POINT('',(-6.,10.5,0.));
#10356=CARTESIAN_POINT('',(-6.,10.5,-0.8));
#10357=CARTESIAN_POINT('',(-4.,10.5,0.));
#10358=CARTESIAN_POINT('',(-4.,10.5,0.));
#10359=CARTESIAN_POINT('',(-4.,10.5,-0.8));
#10360=CARTESIAN_POINT('Origin',(-4.,-2.,-0.8));
#10361=CARTESIAN_POINT('',(-4.,-2.,-0.8));
#10362=CARTESIAN_POINT('',(-4.,-2.,-0.8));
#10363=CARTESIAN_POINT('',(-4.,-2.,0.));
#10364=CARTESIAN_POINT('',(-4.,-2.,0.));
#10365=CARTESIAN_POINT('',(-4.,-2.,-0.8));
#10366=CARTESIAN_POINT('Origin',(-6.,-2.,-0.8));
#10367=CARTESIAN_POINT('',(-6.,-2.,-0.8));
#10368=CARTESIAN_POINT('',(-6.,-2.,-0.8));
#10369=CARTESIAN_POINT('',(-6.,-2.,0.));
#10370=CARTESIAN_POINT('',(-6.,-2.,0.));
#10371=CARTESIAN_POINT('',(-6.,-2.,-0.8));
#10372=CARTESIAN_POINT('Origin',(-6.,10.5,-0.8));
#10373=CARTESIAN_POINT('',(-6.,10.5,-0.8));
#10374=CARTESIAN_POINT('',(-6.,10.5,0.));
#10375=CARTESIAN_POINT('Origin',(-5.,4.25,0.));
#10376=CARTESIAN_POINT('Origin',(-5.,4.25,-0.8));
#10377=CARTESIAN_POINT('',(0.,0.,0.));
#10378=CARTESIAN_POINT('Origin',(11.,10.5,-0.8));
#10379=CARTESIAN_POINT('',(11.,10.5,-0.8));
#10380=CARTESIAN_POINT('',(9.,10.5,-0.8));
#10381=CARTESIAN_POINT('',(11.,10.5,-0.8));
#10382=CARTESIAN_POINT('',(9.,10.5,0.));
#10383=CARTESIAN_POINT('',(9.,10.5,-0.8));
#10384=CARTESIAN_POINT('',(11.,10.5,0.));
#10385=CARTESIAN_POINT('',(11.,10.5,0.));
#10386=CARTESIAN_POINT('',(11.,10.5,-0.8));
#10387=CARTESIAN_POINT('Origin',(11.,-2.,-0.8));
#10388=CARTESIAN_POINT('',(11.,-2.,-0.8));
#10389=CARTESIAN_POINT('',(11.,-2.,-0.8));
#10390=CARTESIAN_POINT('',(11.,-2.,0.));
#10391=CARTESIAN_POINT('',(11.,-2.,0.));
#10392=CARTESIAN_POINT('',(11.,-2.,-0.8));
#10393=CARTESIAN_POINT('Origin',(9.,-2.,-0.8));
#10394=CARTESIAN_POINT('',(9.,-2.,-0.8));
#10395=CARTESIAN_POINT('',(9.,-2.,-0.8));
#10396=CARTESIAN_POINT('',(9.,-2.,0.));
#10397=CARTESIAN_POINT('',(9.,-2.,0.));
#10398=CARTESIAN_POINT('',(9.,-2.,-0.8));
#10399=CARTESIAN_POINT('Origin',(9.,10.5,-0.8));
#10400=CARTESIAN_POINT('',(9.,10.5,-0.8));
#10401=CARTESIAN_POINT('',(9.,10.5,0.));
#10402=CARTESIAN_POINT('Origin',(10.,4.25,0.));
#10403=CARTESIAN_POINT('Origin',(10.,4.25,-0.8));
#10404=CARTESIAN_POINT('',(0.,0.,0.));
#10405=CARTESIAN_POINT('',(0.,0.,0.));
#10406=CARTESIAN_POINT('Origin',(0.,0.,0.));
#10407=CARTESIAN_POINT('',(-1.88531,-0.410863395882378,-2.3088388569005E-16));
#10408=CARTESIAN_POINT('',(-2.3088388569005E-16,-0.410863395882378,1.88531));
#10409=CARTESIAN_POINT('Origin',(0.,-0.410863395882378,0.));
#10410=CARTESIAN_POINT('Origin',(0.,-0.410863395882378,0.));
#10411=CARTESIAN_POINT('',(-2.3088388569005E-16,0.410863395882378,1.88531));
#10412=CARTESIAN_POINT('Origin',(-2.35744508835865E-16,0.,1.925));
#10413=CARTESIAN_POINT('',(-1.88531,0.410863395882378,2.3088388569005E-16));
#10414=CARTESIAN_POINT('Origin',(0.,0.410863395882378,0.));
#10415=CARTESIAN_POINT('Origin',(0.,0.410863395882378,0.));
#10416=CARTESIAN_POINT('Origin',(0.,0.,0.));
#10417=CARTESIAN_POINT('',(-1.88531,0.75,-2.3088388569005E-16));
#10418=CARTESIAN_POINT('',(-1.88531,0.,-2.3088388569005E-16));
#10419=CARTESIAN_POINT('Origin',(0.,0.75,0.));
#10420=CARTESIAN_POINT('Origin',(0.,0.,0.));
#10421=CARTESIAN_POINT('',(-1.25,-0.65,-1.53080849893419E-16));
#10422=CARTESIAN_POINT('Origin',(0.,-0.65,0.));
#10423=CARTESIAN_POINT('',(-1.25,0.65,-1.53080849893419E-16));
#10424=CARTESIAN_POINT('',(-1.25,0.,-1.53080849893419E-16));
#10425=CARTESIAN_POINT('Origin',(0.,0.65,0.));
#10426=CARTESIAN_POINT('Origin',(0.,0.7,0.));
#10427=CARTESIAN_POINT('',(-1.35,0.75,-1.65327317884893E-16));
#10428=CARTESIAN_POINT('',(-1.3,0.7,-1.59204083889156E-16));
#10429=CARTESIAN_POINT('Origin',(0.,0.75,0.));
#10430=CARTESIAN_POINT('Origin',(1.88531,0.75,0.));
#10431=CARTESIAN_POINT('Origin',(0.,0.,0.));
#10432=CARTESIAN_POINT('',(-1.88531,-0.75,-2.3088388569005E-16));
#10433=CARTESIAN_POINT('Origin',(0.,-0.75,0.));
#10434=CARTESIAN_POINT('',(-1.88531,0.,-2.3088388569005E-16));
#10435=CARTESIAN_POINT('Origin',(1.35,-0.75,0.));
#10436=CARTESIAN_POINT('',(-1.35,-0.75,-1.65327317884893E-16));
#10437=CARTESIAN_POINT('Origin',(0.,-0.75,0.));
#10438=CARTESIAN_POINT('Origin',(0.,-0.7,0.));
#10439=CARTESIAN_POINT('',(-1.3,-0.7,-1.59204083889156E-16));
#10440=CARTESIAN_POINT('',(0.,0.,0.));
#10441=CARTESIAN_POINT('Origin',(0.,0.,0.));
#10442=CARTESIAN_POINT('',(-1.96469,0.410863395882378,-2.40605131981681E-16));
#10443=CARTESIAN_POINT('',(-2.40605131981681E-16,0.410863395882378,1.96469));
#10444=CARTESIAN_POINT('Origin',(0.,0.410863395882378,0.));
#10445=CARTESIAN_POINT('Origin',(0.,0.410863395882378,0.));
#10446=CARTESIAN_POINT('',(-2.40605131981681E-16,-0.410863395882378,1.96469));
#10447=CARTESIAN_POINT('Origin',(-2.35744508835865E-16,0.,1.925));
#10448=CARTESIAN_POINT('',(-1.96469,-0.410863395882378,2.40605131981681E-16));
#10449=CARTESIAN_POINT('Origin',(0.,-0.410863395882378,0.));
#10450=CARTESIAN_POINT('Origin',(0.,-0.410863395882378,0.));
#10451=CARTESIAN_POINT('Origin',(0.,0.,0.));
#10452=CARTESIAN_POINT('',(-1.96469,-0.75,-2.40605131981681E-16));
#10453=CARTESIAN_POINT('Origin',(0.,-0.75,0.));
#10454=CARTESIAN_POINT('',(-1.96469,0.,-2.40605131981681E-16));
#10455=CARTESIAN_POINT('Origin',(2.5,0.75,0.));
#10456=CARTESIAN_POINT('',(-2.5,0.75,-3.06161699786838E-16));
#10457=CARTESIAN_POINT('Origin',(0.,0.75,0.));
#10458=CARTESIAN_POINT('',(-1.96469,0.75,-2.40605131981681E-16));
#10459=CARTESIAN_POINT('Origin',(0.,0.75,0.));
#10460=CARTESIAN_POINT('Origin',(0.,0.7,0.));
#10461=CARTESIAN_POINT('',(-2.6,0.65,-3.18408167778312E-16));
#10462=CARTESIAN_POINT('Origin',(0.,0.65,0.));
#10463=CARTESIAN_POINT('',(-2.55,0.7,-3.12284933782575E-16));
#10464=CARTESIAN_POINT('Origin',(0.,0.,0.));
#10465=CARTESIAN_POINT('',(-2.6,-0.65,-3.18408167778312E-16));
#10466=CARTESIAN_POINT('Origin',(0.,-0.65,0.));
#10467=CARTESIAN_POINT('',(-2.6,0.,-3.18408167778312E-16));
#10468=CARTESIAN_POINT('Origin',(0.,-0.7,0.));
#10469=CARTESIAN_POINT('',(-2.5,-0.75,-3.06161699786838E-16));
#10470=CARTESIAN_POINT('Origin',(0.,-0.75,0.));
#10471=CARTESIAN_POINT('',(-2.55,-0.7,-3.12284933782575E-16));
#10472=CARTESIAN_POINT('Origin',(1.96469,-0.75,0.));
#10473=CARTESIAN_POINT('Origin',(0.,0.,0.));
#10474=CARTESIAN_POINT('',(-1.96469,0.,-2.40605131981681E-16));
#10475=CARTESIAN_POINT('',(0.,0.,0.));
#10476=CARTESIAN_POINT('Origin',(1.925,0.,0.));
#10477=CARTESIAN_POINT('',(1.925,-2.97627328869245E-33,0.3969));
#10478=CARTESIAN_POINT('',(1.925,-2.97627328869245E-33,-0.3969));
#10479=CARTESIAN_POINT('Origin',(1.925,0.,0.));
#10480=CARTESIAN_POINT('Origin',(1.47463555300403,0.,-1.23736614864659));
#10481=CARTESIAN_POINT('',(1.72975795528862,-2.97627328869245E-33,-0.933323109172666));
#10482=CARTESIAN_POINT('',(1.21951315071945,-2.97627328869245E-33,-1.54140918812051));
#10483=CARTESIAN_POINT('Origin',(1.47463555300403,0.,-1.23736614864659));
#10484=CARTESIAN_POINT('Origin',(0.334272742008841,0.,-1.8957549245485));
#10485=CARTESIAN_POINT('',(0.725142939179386,1.05214622327121E-34,-1.8268339628325));
#10486=CARTESIAN_POINT('',(-0.0565974551617042,-6.05776119971203E-33,-1.96467588626451));
#10487=CARTESIAN_POINT('Origin',(0.334272742008841,0.,-1.8957549245485));
#10488=CARTESIAN_POINT('Origin',(-0.9625,0.,-1.66709890228504));
#10489=CARTESIAN_POINT('',(-0.618774517237956,-2.97627328869245E-33,-1.86554890228504));
#10490=CARTESIAN_POINT('',(-1.30622548276204,-2.97627328869245E-33,-1.46864890228504));
#10491=CARTESIAN_POINT('Origin',(-0.9625,0.,-1.66709890228504));
#10492=CARTESIAN_POINT('Origin',(-1.80890829501287,0.,-0.658388775901913));
#10493=CARTESIAN_POINT('',(-1.67316050012692,1.05214622327121E-34,-1.03135277709184));
#10494=CARTESIAN_POINT('',(-1.94465608989883,-6.05776119971203E-33,-0.285424774711986));
#10495=CARTESIAN_POINT('Origin',(-1.80890829501287,0.,-0.658388775901913));
#10496=CARTESIAN_POINT('Origin',(-1.80890829501287,0.,0.658388775901912));
#10497=CARTESIAN_POINT('',(-1.94465608989883,-9.13924911073161E-33,0.285424774711985));
#10498=CARTESIAN_POINT('',(-1.67316050012692,3.1867025333467E-33,1.03135277709184));
#10499=CARTESIAN_POINT('Origin',(-1.80890829501287,0.,0.658388775901912));
#10500=CARTESIAN_POINT('Origin',(-0.962500000000001,0.,1.66709890228504));
#10501=CARTESIAN_POINT('',(-1.30622548276204,-2.97627328869245E-33,1.46864890228504));
#10502=CARTESIAN_POINT('',(-0.618774517237957,-2.97627328869245E-33,1.86554890228504));
#10503=CARTESIAN_POINT('Origin',(-0.962500000000001,0.,1.66709890228504));
#10504=CARTESIAN_POINT('Origin',(0.33427274200884,0.,1.8957549245485));
#10505=CARTESIAN_POINT('',(-0.0565974551617051,-2.97627328869245E-33,1.96467588626451));
#10506=CARTESIAN_POINT('',(0.725142939179386,-2.97627328869245E-33,1.8268339628325));
#10507=CARTESIAN_POINT('Origin',(0.33427274200884,0.,1.8957549245485));
#10508=CARTESIAN_POINT('Origin',(1.47463555300403,0.,1.23736614864659));
#10509=CARTESIAN_POINT('',(1.21951315071944,-6.05776119971203E-33,1.54140918812051));
#10510=CARTESIAN_POINT('',(1.72975795528862,1.05214622327122E-34,0.933323109172667));
#10511=CARTESIAN_POINT('Origin',(1.47463555300403,0.,1.23736614864659));
#10512=CARTESIAN_POINT('',(0.,0.,0.));
#10513=CARTESIAN_POINT('Origin',(1.47463555300403,0.,1.23736614864659));
#10514=CARTESIAN_POINT('',(1.16188454446795,-0.07938,1.49479506783723));
#10515=CARTESIAN_POINT('',(1.67384490577674,-0.07938,0.884664467981643));
#10516=CARTESIAN_POINT('Ctrl Pts',(1.16188454446795,-0.07938,1.49479506783723));
#10517=CARTESIAN_POINT('Ctrl Pts',(1.16869700612251,-0.123392992551698,
1.48949983100074));
#10518=CARTESIAN_POINT('Ctrl Pts',(1.18135446441955,-0.166529565724166,
1.47962830891229));
#10519=CARTESIAN_POINT('Ctrl Pts',(1.21282145231718,-0.237213819614884,
1.45388393800011));
#10520=CARTESIAN_POINT('Ctrl Pts',(1.22989120215288,-0.266247928944116,
1.4395843844684));
#10521=CARTESIAN_POINT('Ctrl Pts',(1.26813946847809,-0.317173992396757,
1.40600777299249));
#10522=CARTESIAN_POINT('Ctrl Pts',(1.28931069477441,-0.339063173951852,
1.38671820696899));
#10523=CARTESIAN_POINT('Ctrl Pts',(1.33224261954459,-0.373566122196588,
1.34549913552853));
#10524=CARTESIAN_POINT('Ctrl Pts',(1.35618281536764,-0.388075792674378,
1.32151296077672));
#10525=CARTESIAN_POINT('Ctrl Pts',(1.40439359896051,-0.407069005705619,
1.27016020894803));
#10526=CARTESIAN_POINT('Ctrl Pts',(1.42864614483643,-0.411552957311693,
1.24277684810113));
#10527=CARTESIAN_POINT('Ctrl Pts',(1.4719780748558,-0.411552957311693,1.19113586482651));
#10528=CARTESIAN_POINT('Ctrl Pts',(1.49473401052622,-0.407069005705619,
1.16249669890816));
#10529=CARTESIAN_POINT('Ctrl Pts',(1.53693488395083,-0.388075792674377,
1.10610103367387));
#10530=CARTESIAN_POINT('Ctrl Pts',(1.55639948343386,-0.373566122196588,
1.07835938768384));
#10531=CARTESIAN_POINT('Ctrl Pts',(1.58953729406031,-0.339063173951852,
1.02892207867768));
#10532=CARTESIAN_POINT('Ctrl Pts',(1.60485746336717,-0.317173992396757,
1.00472289289232));
#10533=CARTESIAN_POINT('Ctrl Pts',(1.63128222892223,-0.266247928944116,
0.961225186280959));
#10534=CARTESIAN_POINT('Ctrl Pts',(1.64240040915267,-0.237213819614884,
0.941931672888549));
#10535=CARTESIAN_POINT('Ctrl Pts',(1.66228948011831,-0.166529565724165,
0.906472276148935));
#10536=CARTESIAN_POINT('Ctrl Pts',(1.66981308703787,-0.123392992551698,
0.892292941263125));
#10537=CARTESIAN_POINT('Ctrl Pts',(1.67384490577674,-0.07938,0.884664467981643));
#10538=CARTESIAN_POINT('',(1.20622598189858,-0.07938,1.54074568637942));
#10539=CARTESIAN_POINT('Origin',(1.47463555300403,-0.07938,1.23736614864659));
#10540=CARTESIAN_POINT('',(1.72679724097776,-0.07938,0.920353018170519));
#10541=CARTESIAN_POINT('Ctrl Pts',(1.72679724097776,-0.0793800000000002,
0.920353018170518));
#10542=CARTESIAN_POINT('Ctrl Pts',(1.72470909046691,-0.10165971810728,0.92427087628551));
#10543=CARTESIAN_POINT('Ctrl Pts',(1.72169532435455,-0.123845306465941,
0.929898398578877));
#10544=CARTESIAN_POINT('Ctrl Pts',(1.70911544962889,-0.192537547974292,
0.952957916220029));
#10545=CARTESIAN_POINT('Ctrl Pts',(1.69580594901181,-0.236239311587943,
0.976785804874841));
#10546=CARTESIAN_POINT('Ctrl Pts',(1.66527150643903,-0.303218781300911,
1.02787962443771));
#10547=CARTESIAN_POINT('Ctrl Pts',(1.64438322958071,-0.3351607303803,1.06123747122987));
#10548=CARTESIAN_POINT('Ctrl Pts',(1.60730731395783,-0.3732673312795,1.11639170354769));
#10549=CARTESIAN_POINT('Ctrl Pts',(1.5873911192195,-0.387903357081022,1.1447096804553));
#10550=CARTESIAN_POINT('Ctrl Pts',(1.54427174765086,-0.40704475551587,1.20224605970712));
#10551=CARTESIAN_POINT('Ctrl Pts',(1.52104964294098,-0.411552957311693,
1.23144933316771));
#10552=CARTESIAN_POINT('Ctrl Pts',(1.47686834938291,-0.411552957311693,
1.284102548491));
#10553=CARTESIAN_POINT('Ctrl Pts',(1.45214121543005,-0.40704475551587,1.31204295246889));
#10554=CARTESIAN_POINT('Ctrl Pts',(1.40296654335764,-0.387903357081022,
1.36449833130133));
#10555=CARTESIAN_POINT('Ctrl Pts',(1.37853719107178,-0.3732673312795,1.38902931937536));
#10556=CARTESIAN_POINT('Ctrl Pts',(1.330659040657,-0.3351607303803,1.43511940046341));
#10557=CARTESIAN_POINT('Ctrl Pts',(1.30143518572334,-0.303218781300911,
1.4614828667669));
#10558=CARTESIAN_POINT('Ctrl Pts',(1.25641984639565,-0.236239311587943,
1.50042577120361));
#10559=CARTESIAN_POINT('Ctrl Pts',(1.23526512743829,-0.192537547974292,
1.51767074004259));
#10560=CARTESIAN_POINT('Ctrl Pts',(1.21474040800595,-0.123845306465941,
1.53406374142061));
#10561=CARTESIAN_POINT('Ctrl Pts',(1.20972171541452,-0.10165971810728,1.53800893064485));
#10562=CARTESIAN_POINT('Ctrl Pts',(1.20622598189858,-0.0793800000000002,
1.54074568637942));
#10563=CARTESIAN_POINT('Origin',(1.47463555300403,-0.07938,1.23736614864659));
#10564=CARTESIAN_POINT('Origin',(0.,-0.27783,0.));
#10565=CARTESIAN_POINT('',(0.731211914226578,-0.07938,1.81499518621871));
#10566=CARTESIAN_POINT('Origin',(0.,-0.07938,0.));
#10567=CARTESIAN_POINT('',(-0.0663495263035324,-0.07938,1.95562678695688));
#10568=CARTESIAN_POINT('Ctrl Pts',(0.73121191422658,-0.0793800000000002,
1.81499518621871));
#10569=CARTESIAN_POINT('Ctrl Pts',(0.727093947478514,-0.10165971810728,
1.81665420238109));
#10570=CARTESIAN_POINT('Ctrl Pts',(0.721167967091869,-0.123845306465941,
1.81902792304693));
#10571=CARTESIAN_POINT('Ctrl Pts',(0.696708851738065,-0.192537547974292,
1.82860635079188));
#10572=CARTESIAN_POINT('Ctrl Pts',(0.671196911157359,-0.236239311587943,
1.83830439039938));
#10573=CARTESIAN_POINT('Ctrl Pts',(0.614963696954177,-0.303218781300911,
1.85781736559878));
#10574=CARTESIAN_POINT('Ctrl Pts',(0.577520337936704,-0.3351607303803,1.86994423321609));
#10575=CARTESIAN_POINT('Ctrl Pts',(0.513666081644577,-0.3732673312795,1.88836288721748));
#10576=CARTESIAN_POINT('Ctrl Pts',(0.48020694664961,-0.387903357081022,
1.89725383285802));
#10577=CARTESIAN_POINT('Ctrl Pts',(0.410191919979371,-0.40704475551587,
1.91361265867928));
#10578=CARTESIAN_POINT('Ctrl Pts',(0.373631253366087,-0.411552957311693,
1.92105678285629));
#10579=CARTESIAN_POINT('Ctrl Pts',(0.305941584526154,-0.411552957311693,
1.932992297788));
#10580=CARTESIAN_POINT('Ctrl Pts',(0.269039755480681,-0.40704475551587,
1.9385015936658));
#10581=CARTESIAN_POINT('Ctrl Pts',(0.197652103622503,-0.387903357081022,
1.94707587521355));
#10582=CARTESIAN_POINT('Ctrl Pts',(0.163169918867575,-0.3732673312795,1.95016481734985));
#10583=CARTESIAN_POINT('Ctrl Pts',(0.09686699474267,-0.3351607303803,1.95469638598893));
#10584=CARTESIAN_POINT('Ctrl Pts',(0.0575341135759475,-0.30321878130091,
1.95610724099344));
#10585=CARTESIAN_POINT('Ctrl Pts',(-0.00198165342826295,-0.236239311587942,
1.95700393417042));
#10586=CARTESIAN_POINT('Ctrl Pts',(-0.0292719606304177,-0.192537547974292,
1.95661635548909));
#10587=CARTESIAN_POINT('Ctrl Pts',(-0.0555320260694991,-0.123845306465941,
1.95598108775736));
#10588=CARTESIAN_POINT('Ctrl Pts',(-0.0619124863920986,-0.10165971810728,
1.95577732462505));
#10589=CARTESIAN_POINT('Ctrl Pts',(-0.0663495263035336,-0.0793800000000002,
1.95562678695688));
#10590=CARTESIAN_POINT('',(-0.606515593706441,-0.07938,1.86038093521056));
#10591=CARTESIAN_POINT('Origin',(0.,-0.07938,0.));
#10592=CARTESIAN_POINT('',(-1.30787935375538,-0.07938,1.45544837954646));
#10593=CARTESIAN_POINT('Ctrl Pts',(-0.60651559370644,-0.0793800000000002,
1.86038093521056));
#10594=CARTESIAN_POINT('Ctrl Pts',(-0.610736534284191,-0.10165971810728,
1.85900483732004));
#10595=CARTESIAN_POINT('Ctrl Pts',(-0.616801896862274,-0.123845306465941,
1.85701406607784));
#10596=CARTESIAN_POINT('Ctrl Pts',(-0.64169556093739,-0.192537547974292,
1.84862955113236));
#10597=CARTESIAN_POINT('Ctrl Pts',(-0.667472620950374,-0.236239311587943,
1.8396599211785));
#10598=CARTESIAN_POINT('Ctrl Pts',(-0.723092460895733,-0.303218781300911,
1.81846171405606));
#10599=CARTESIAN_POINT('Ctrl Pts',(-0.759570738251496,-0.3351607303803,
1.80368330636526));
#10600=CARTESIAN_POINT('Ctrl Pts',(-0.820325219032771,-0.3732673312795,
1.77674808914243));
#10601=CARTESIAN_POINT('Ctrl Pts',(-0.851671393163369,-0.387903357081022,
1.76205183123884));
#10602=CARTESIAN_POINT('Ctrl Pts',(-0.915821265825857,-0.40704475551587,
1.72957862721967));
#10603=CARTESIAN_POINT('Ctrl Pts',(-0.948613352107641,-0.411552957311693,
1.71178041367846));
#10604=CARTESIAN_POINT('Ctrl Pts',(-1.00813864789236,-0.411552957311693,
1.67741346813356));
#10605=CARTESIAN_POINT('Ctrl Pts',(-1.03994839610192,-0.40704475551587,
1.65791379514105));
#10606=CARTESIAN_POINT('Ctrl Pts',(-1.10014595205605,-0.387903357081022,
1.61859497777538));
#10607=CARTESIAN_POINT('Ctrl Pts',(-1.12854637180642,-0.3732673312795,1.59879652361863));
#10608=CARTESIAN_POINT('Ctrl Pts',(-1.18225019456848,-0.3351607303803,1.55964920847973));
#10609=CARTESIAN_POINT('Ctrl Pts',(-1.21328780973407,-0.30321878130091,
1.53544729744874));
#10610=CARTESIAN_POINT('Ctrl Pts',(-1.25945591558947,-0.236239311587942,
1.49787820666285));
#10611=CARTESIAN_POINT('Ctrl Pts',(-1.28011237299855,-0.192537547974292,
1.48003943283366));
#10612=CARTESIAN_POINT('Ctrl Pts',(-1.29982040797731,-0.12384530646594,
1.46267314482408));
#10613=CARTESIAN_POINT('Ctrl Pts',(-1.30457714773522,-0.10165971810728,
1.45841577236939));
#10614=CARTESIAN_POINT('Ctrl Pts',(-1.30787935375538,-0.0793800000000002,
1.45544837954646));
#10615=CARTESIAN_POINT('',(-1.66044771467423,-0.07938,1.03527376878636));
#10616=CARTESIAN_POINT('Origin',(0.,-0.07938,0.));
#10617=CARTESIAN_POINT('',(-1.93743789612516,-0.07938,0.274249499839291));
#10618=CARTESIAN_POINT('Ctrl Pts',(-1.66044771467423,-0.0793800000000002,
1.03527376878636));
#10619=CARTESIAN_POINT('Ctrl Pts',(-1.66279660407481,-0.10165971810728,
1.03150644833954));
#10620=CARTESIAN_POINT('Ctrl Pts',(-1.66616329828505,-0.123845306465941,
1.02608268917849));
#10621=CARTESIAN_POINT('Ctrl Pts',(-1.67984348899847,-0.192537547974292,
1.00365843926907));
#10622=CARTESIAN_POINT('Ctrl Pts',(-1.69382429558355,-0.236239311587943,
0.980218129295584));
#10623=CARTESIAN_POINT('Ctrl Pts',(-1.72280562001498,-0.303218781300911,
0.928227616555729));
#10624=CARTESIAN_POINT('Ctrl Pts',(-1.74125022432338,-0.3351607303803,0.893458914759057));
#10625=CARTESIAN_POINT('Ctrl Pts',(-1.7704772328254,-0.3732673312795,0.833773113802161));
#10626=CARTESIAN_POINT('Ctrl Pts',(-1.785043222842,-0.387903357081022,0.802366194758251));
#10627=CARTESIAN_POINT('Ctrl Pts',(-1.81331150313154,-0.407044755515871,
0.736255533958675));
#10628=CARTESIAN_POINT('Ctrl Pts',(-1.82699122746714,-0.411552957311693,
0.701542964620283));
#10629=CARTESIAN_POINT('Ctrl Pts',(-1.850499602749,-0.411552957311693,0.636954234365294));
#10630=CARTESIAN_POINT('Ctrl Pts',(-1.86233313540942,-0.40704475551587,
0.60156970621039));
#10631=CARTESIAN_POINT('Ctrl Pts',(-1.88317349000725,-0.387903357081022,
0.53275550155669));
#10632=CARTESIAN_POINT('Ctrl Pts',(-1.89220327271636,-0.3732673312795,0.499333567842125));
#10633=CARTESIAN_POINT('Ctrl Pts',(-1.9081793785937,-0.3351607303803,0.434824832752687));
#10634=CARTESIAN_POINT('Ctrl Pts',(-1.91639888267751,-0.30321878130091,
0.396334498831876));
#10635=CARTESIAN_POINT('Ctrl Pts',(-1.92761675755301,-0.236239311587942,
0.337878619195771));
#10636=CARTESIAN_POINT('Ctrl Pts',(-1.93197397917636,-0.192537547974292,
0.310935610749289));
#10637=CARTESIAN_POINT('Ctrl Pts',(-1.93590837509782,-0.12384530646594,
0.284964181626328));
#10638=CARTESIAN_POINT('Ctrl Pts',(-1.93681566289304,-0.10165971810728,
0.278645271736243));
#10639=CARTESIAN_POINT('Ctrl Pts',(-1.93743789612516,-0.0793800000000002,
0.27424949983929));
#10640=CARTESIAN_POINT('',(-1.956752,-0.07938,2.39633007352518E-16));
#10641=CARTESIAN_POINT('Origin',(0.,-0.07938,0.));
#10642=CARTESIAN_POINT('',(-1.956752,-0.47628,2.39633007352518E-16));
#10643=CARTESIAN_POINT('',(-1.956752,-0.27783,2.39633007352518E-16));
#10644=CARTESIAN_POINT('Origin',(0.,-0.47628,0.));
#10645=CARTESIAN_POINT('',(-1.93743789612516,-0.07938,-0.274249499839292));
#10646=CARTESIAN_POINT('Origin',(0.,-0.07938,0.));
#10647=CARTESIAN_POINT('',(-1.66044771467423,-0.07938,-1.03527376878636));
#10648=CARTESIAN_POINT('Ctrl Pts',(-1.93743789612516,-0.0793800000000002,
-0.27424949983929));
#10649=CARTESIAN_POINT('Ctrl Pts',(-1.93681566289304,-0.10165971810728,
-0.278645271736244));
#10650=CARTESIAN_POINT('Ctrl Pts',(-1.93590837509782,-0.123845306465941,
-0.284964181626328));
#10651=CARTESIAN_POINT('Ctrl Pts',(-1.93197397917636,-0.192537547974292,
-0.310935610749289));
#10652=CARTESIAN_POINT('Ctrl Pts',(-1.92761675755301,-0.236239311587942,
-0.337878619195772));
#10653=CARTESIAN_POINT('Ctrl Pts',(-1.91639888267751,-0.303218781300911,
-0.396334498831877));
#10654=CARTESIAN_POINT('Ctrl Pts',(-1.9081793785937,-0.3351607303803,-0.434824832752687));
#10655=CARTESIAN_POINT('Ctrl Pts',(-1.89220327271636,-0.3732673312795,-0.499333567842125));
#10656=CARTESIAN_POINT('Ctrl Pts',(-1.88317349000725,-0.387903357081022,
-0.53275550155669));
#10657=CARTESIAN_POINT('Ctrl Pts',(-1.86233313540942,-0.40704475551587,
-0.601569706210391));
#10658=CARTESIAN_POINT('Ctrl Pts',(-1.850499602749,-0.411552957311693,-0.636954234365295));
#10659=CARTESIAN_POINT('Ctrl Pts',(-1.82699122746714,-0.411552957311693,
-0.701542964620284));
#10660=CARTESIAN_POINT('Ctrl Pts',(-1.81331150313154,-0.40704475551587,
-0.736255533958675));
#10661=CARTESIAN_POINT('Ctrl Pts',(-1.785043222842,-0.387903357081022,-0.802366194758251));
#10662=CARTESIAN_POINT('Ctrl Pts',(-1.7704772328254,-0.3732673312795,-0.833773113802161));
#10663=CARTESIAN_POINT('Ctrl Pts',(-1.74125022432338,-0.3351607303803,-0.893458914759057));
#10664=CARTESIAN_POINT('Ctrl Pts',(-1.72280562001498,-0.303218781300911,
-0.92822761655573));
#10665=CARTESIAN_POINT('Ctrl Pts',(-1.69382429558355,-0.236239311587942,
-0.980218129295584));
#10666=CARTESIAN_POINT('Ctrl Pts',(-1.67984348899847,-0.192537547974292,
-1.00365843926907));
#10667=CARTESIAN_POINT('Ctrl Pts',(-1.66616329828505,-0.123845306465941,
-1.02608268917849));
#10668=CARTESIAN_POINT('Ctrl Pts',(-1.66279660407481,-0.10165971810728,
-1.03150644833954));
#10669=CARTESIAN_POINT('Ctrl Pts',(-1.66044771467423,-0.0793800000000001,
-1.03527376878636));
#10670=CARTESIAN_POINT('',(-1.30787935375538,-0.07938,-1.45544837954646));
#10671=CARTESIAN_POINT('Origin',(0.,-0.07938,0.));
#10672=CARTESIAN_POINT('',(-0.60651559370644,-0.07938,-1.86038093521056));
#10673=CARTESIAN_POINT('Ctrl Pts',(-1.30787935375538,-0.0793800000000002,
-1.45544837954646));
#10674=CARTESIAN_POINT('Ctrl Pts',(-1.30457714773522,-0.10165971810728,
-1.45841577236939));
#10675=CARTESIAN_POINT('Ctrl Pts',(-1.29982040797731,-0.123845306465941,
-1.46267314482408));
#10676=CARTESIAN_POINT('Ctrl Pts',(-1.28011237299855,-0.192537547974292,
-1.48003943283366));
#10677=CARTESIAN_POINT('Ctrl Pts',(-1.25945591558947,-0.236239311587942,
-1.49787820666285));
#10678=CARTESIAN_POINT('Ctrl Pts',(-1.21328780973407,-0.303218781300911,
-1.53544729744874));
#10679=CARTESIAN_POINT('Ctrl Pts',(-1.18225019456848,-0.3351607303803,-1.55964920847973));
#10680=CARTESIAN_POINT('Ctrl Pts',(-1.12854637180642,-0.3732673312795,-1.59879652361863));
#10681=CARTESIAN_POINT('Ctrl Pts',(-1.10014595205605,-0.387903357081022,
-1.61859497777538));
#10682=CARTESIAN_POINT('Ctrl Pts',(-1.03994839610192,-0.40704475551587,
-1.65791379514105));
#10683=CARTESIAN_POINT('Ctrl Pts',(-1.00813864789236,-0.411552957311693,
-1.67741346813356));
#10684=CARTESIAN_POINT('Ctrl Pts',(-0.948613352107639,-0.411552957311693,
-1.71178041367846));
#10685=CARTESIAN_POINT('Ctrl Pts',(-0.915821265825855,-0.40704475551587,
-1.72957862721967));
#10686=CARTESIAN_POINT('Ctrl Pts',(-0.851671393163367,-0.387903357081022,
-1.76205183123885));
#10687=CARTESIAN_POINT('Ctrl Pts',(-0.820325219032769,-0.3732673312795,
-1.77674808914243));
#10688=CARTESIAN_POINT('Ctrl Pts',(-0.759570738251494,-0.3351607303803,
-1.80368330636526));
#10689=CARTESIAN_POINT('Ctrl Pts',(-0.723092460895731,-0.303218781300911,
-1.81846171405606));
#10690=CARTESIAN_POINT('Ctrl Pts',(-0.667472620950373,-0.236239311587942,
-1.8396599211785));
#10691=CARTESIAN_POINT('Ctrl Pts',(-0.641695560937389,-0.192537547974292,
-1.84862955113236));
#10692=CARTESIAN_POINT('Ctrl Pts',(-0.616801896862272,-0.123845306465941,
-1.85701406607784));
#10693=CARTESIAN_POINT('Ctrl Pts',(-0.610736534284189,-0.10165971810728,
-1.85900483732004));
#10694=CARTESIAN_POINT('Ctrl Pts',(-0.606515593706439,-0.0793800000000002,
-1.86038093521056));
#10695=CARTESIAN_POINT('',(-0.0663495263035315,-0.07938,-1.95562678695688));
#10696=CARTESIAN_POINT('Origin',(0.,-0.07938,0.));
#10697=CARTESIAN_POINT('',(0.731211914226579,-0.07938,-1.81499518621871));
#10698=CARTESIAN_POINT('Ctrl Pts',(-0.0663495263035327,-0.0793800000000002,
-1.95562678695688));
#10699=CARTESIAN_POINT('Ctrl Pts',(-0.0619124863920977,-0.10165971810728,
-1.95577732462505));
#10700=CARTESIAN_POINT('Ctrl Pts',(-0.0555320260694982,-0.123845306465941,
-1.95598108775736));
#10701=CARTESIAN_POINT('Ctrl Pts',(-0.0292719606304167,-0.192537547974292,
-1.95661635548909));
#10702=CARTESIAN_POINT('Ctrl Pts',(-0.00198165342826177,-0.236239311587943,
-1.95700393417042));
#10703=CARTESIAN_POINT('Ctrl Pts',(0.0575341135759488,-0.303218781300911,
-1.95610724099344));
#10704=CARTESIAN_POINT('Ctrl Pts',(0.0968669947426714,-0.3351607303803,
-1.95469638598893));
#10705=CARTESIAN_POINT('Ctrl Pts',(0.163169918867576,-0.3732673312795,-1.95016481734985));
#10706=CARTESIAN_POINT('Ctrl Pts',(0.197652103622504,-0.387903357081022,
-1.94707587521355));
#10707=CARTESIAN_POINT('Ctrl Pts',(0.269039755480682,-0.40704475551587,
-1.9385015936658));
#10708=CARTESIAN_POINT('Ctrl Pts',(0.305941584526155,-0.411552957311693,
-1.93299229778799));
#10709=CARTESIAN_POINT('Ctrl Pts',(0.373631253366089,-0.411552957311693,
-1.92105678285629));
#10710=CARTESIAN_POINT('Ctrl Pts',(0.410191919979372,-0.40704475551587,
-1.91361265867928));
#10711=CARTESIAN_POINT('Ctrl Pts',(0.480206946649611,-0.387903357081022,
-1.89725383285802));
#10712=CARTESIAN_POINT('Ctrl Pts',(0.513666081644578,-0.3732673312795,-1.88836288721748));
#10713=CARTESIAN_POINT('Ctrl Pts',(0.577520337936705,-0.3351607303803,-1.86994423321609));
#10714=CARTESIAN_POINT('Ctrl Pts',(0.614963696954178,-0.30321878130091,
-1.85781736559878));
#10715=CARTESIAN_POINT('Ctrl Pts',(0.67119691115736,-0.236239311587942,
-1.83830439039938));
#10716=CARTESIAN_POINT('Ctrl Pts',(0.696708851738067,-0.192537547974292,
-1.82860635079188));
#10717=CARTESIAN_POINT('Ctrl Pts',(0.721167967091869,-0.123845306465941,
-1.81902792304693));
#10718=CARTESIAN_POINT('Ctrl Pts',(0.727093947478515,-0.10165971810728,
-1.81665420238109));
#10719=CARTESIAN_POINT('Ctrl Pts',(0.73121191422658,-0.0793800000000002,
-1.81499518621871));
#10720=CARTESIAN_POINT('',(1.20622598189858,-0.07938,-1.54074568637942));
#10721=CARTESIAN_POINT('Origin',(0.,-0.07938,0.));
#10722=CARTESIAN_POINT('',(1.72679724097776,-0.07938,-0.920353018170518));
#10723=CARTESIAN_POINT('Ctrl Pts',(1.20622598189858,-0.0793800000000002,
-1.54074568637942));
#10724=CARTESIAN_POINT('Ctrl Pts',(1.20972171541452,-0.10165971810728,-1.53800893064485));
#10725=CARTESIAN_POINT('Ctrl Pts',(1.21474040800596,-0.123845306465941,
-1.53406374142061));
#10726=CARTESIAN_POINT('Ctrl Pts',(1.23526512743829,-0.192537547974292,
-1.51767074004259));
#10727=CARTESIAN_POINT('Ctrl Pts',(1.25641984639565,-0.236239311587942,
-1.50042577120361));
#10728=CARTESIAN_POINT('Ctrl Pts',(1.30143518572334,-0.303218781300911,
-1.4614828667669));
#10729=CARTESIAN_POINT('Ctrl Pts',(1.330659040657,-0.3351607303803,-1.43511940046341));
#10730=CARTESIAN_POINT('Ctrl Pts',(1.37853719107178,-0.3732673312795,-1.38902931937536));
#10731=CARTESIAN_POINT('Ctrl Pts',(1.40296654335764,-0.387903357081022,
-1.36449833130133));
#10732=CARTESIAN_POINT('Ctrl Pts',(1.45214121543005,-0.40704475551587,-1.31204295246889));
#10733=CARTESIAN_POINT('Ctrl Pts',(1.47686834938291,-0.411552957311693,
-1.284102548491));
#10734=CARTESIAN_POINT('Ctrl Pts',(1.52104964294098,-0.411552957311693,
-1.23144933316771));
#10735=CARTESIAN_POINT('Ctrl Pts',(1.54427174765086,-0.407044755515871,
-1.20224605970712));
#10736=CARTESIAN_POINT('Ctrl Pts',(1.5873911192195,-0.387903357081022,-1.1447096804553));
#10737=CARTESIAN_POINT('Ctrl Pts',(1.60730731395783,-0.3732673312795,-1.11639170354769));
#10738=CARTESIAN_POINT('Ctrl Pts',(1.64438322958071,-0.3351607303803,-1.06123747122987));
#10739=CARTESIAN_POINT('Ctrl Pts',(1.66527150643903,-0.303218781300911,
-1.02787962443771));
#10740=CARTESIAN_POINT('Ctrl Pts',(1.69580594901181,-0.236239311587943,
-0.976785804874841));
#10741=CARTESIAN_POINT('Ctrl Pts',(1.70911544962889,-0.192537547974292,
-0.952957916220028));
#10742=CARTESIAN_POINT('Ctrl Pts',(1.72169532435455,-0.123845306465941,
-0.929898398578876));
#10743=CARTESIAN_POINT('Ctrl Pts',(1.72470909046691,-0.10165971810728,-0.924270876285509));
#10744=CARTESIAN_POINT('Ctrl Pts',(1.72679724097776,-0.0793800000000002,
-0.920353018170518));
#10745=CARTESIAN_POINT('',(1.91439494746182,-0.07938,-0.404932555664102));
#10746=CARTESIAN_POINT('Origin',(0.,-0.07938,0.));
#10747=CARTESIAN_POINT('',(1.91439494746182,-0.07938,0.404932555664102));
#10748=CARTESIAN_POINT('Ctrl Pts',(1.91439494746182,-0.0793800000000002,
-0.404932555664103));
#10749=CARTESIAN_POINT('Ctrl Pts',(1.91531368201941,-0.10165971810728,-0.400589064950645));
#10750=CARTESIAN_POINT('Ctrl Pts',(1.91662230483958,-0.123845306465941,
-0.394340921253764));
#10751=CARTESIAN_POINT('Ctrl Pts',(1.92180793393594,-0.192537547974292,
-0.368590118298695));
#10752=CARTESIAN_POINT('Ctrl Pts',(1.92692853653984,-0.236239311587943,
-0.341781714515643));
#10753=CARTESIAN_POINT('Ctrl Pts',(1.9363802706298,-0.303218781300911,-0.283014416607319));
#10754=CARTESIAN_POINT('Ctrl Pts',(1.94182093281998,-0.3351607303803,-0.244034097885537));
#10755=CARTESIAN_POINT('Ctrl Pts',(1.94887159083919,-0.3732673312795,-0.177951565523803));
#10756=CARTESIAN_POINT('Ctrl Pts',(1.95181734521941,-0.387903357081022,
-0.143456853463462));
#10757=CARTESIAN_POINT('Ctrl Pts',(1.95576966192778,-0.40704475551587,-0.071664832078622));
#10758=CARTESIAN_POINT('Ctrl Pts',(1.956752,-0.411552957311693,-0.0343669455449008));
#10759=CARTESIAN_POINT('Ctrl Pts',(1.956752,-0.411552957311693,0.0343669455449008));
#10760=CARTESIAN_POINT('Ctrl Pts',(1.95576966192778,-0.40704475551587,0.0716648320786219));
#10761=CARTESIAN_POINT('Ctrl Pts',(1.95181734521941,-0.387903357081022,
0.143456853463462));
#10762=CARTESIAN_POINT('Ctrl Pts',(1.94887159083919,-0.3732673312795,0.177951565523803));
#10763=CARTESIAN_POINT('Ctrl Pts',(1.94182093281998,-0.3351607303803,0.244034097885537));
#10764=CARTESIAN_POINT('Ctrl Pts',(1.9363802706298,-0.303218781300911,0.283014416607319));
#10765=CARTESIAN_POINT('Ctrl Pts',(1.92692853653984,-0.236239311587943,
0.341781714515643));
#10766=CARTESIAN_POINT('Ctrl Pts',(1.92180793393594,-0.192537547974292,
0.368590118298695));
#10767=CARTESIAN_POINT('Ctrl Pts',(1.91662230483958,-0.123845306465941,
0.394340921253764));
#10768=CARTESIAN_POINT('Ctrl Pts',(1.91531368201941,-0.10165971810728,0.400589064950645));
#10769=CARTESIAN_POINT('Ctrl Pts',(1.91439494746182,-0.0793800000000002,
0.404932555664103));
#10770=CARTESIAN_POINT('Origin',(0.,-0.07938,0.));
#10771=CARTESIAN_POINT('Origin',(0.,-0.07938,0.));
#10772=CARTESIAN_POINT('',(0.71358822996475,-0.07938,1.75361906569237));
#10773=CARTESIAN_POINT('Origin',(0.,-0.07938,0.));
#10774=CARTESIAN_POINT('Origin',(0.33427274200884,-0.07938,1.8957549245485));
#10775=CARTESIAN_POINT('Origin',(0.33427274200884,0.,1.8957549245485));
#10776=CARTESIAN_POINT('',(-0.070780549790825,-0.07938,1.89192444438865));
#10777=CARTESIAN_POINT('Ctrl Pts',(-0.0707805497908251,-0.07938,1.89192444438865));
#10778=CARTESIAN_POINT('Ctrl Pts',(-0.0621581887675352,-0.123392992551698,
1.89224702357808));
#10779=CARTESIAN_POINT('Ctrl Pts',(-0.0461167210878756,-0.166529565724166,
1.89282105630055));
#10780=CARTESIAN_POINT('Ctrl Pts',(-0.00546344722567869,-0.237213819614884,
1.89332631395644));
#10781=CARTESIAN_POINT('Ctrl Pts',(0.0168043156156246,-0.266247928944116,
1.89334444412923));
#10782=CARTESIAN_POINT('Ctrl Pts',(0.0676868173249578,-0.317173992396757,
1.89220877917518));
#10783=CARTESIAN_POINT('Ctrl Pts',(0.0963040116194015,-0.339063173951852,
1.89104071625784));
#10784=CARTESIAN_POINT('Ctrl Pts',(0.155686882426711,-0.373566122196588,
1.88706118493262));
#10785=CARTESIAN_POINT('Ctrl Pts',(0.189444152338378,-0.388075792674378,
1.88407517030084));
#10786=CARTESIAN_POINT('Ctrl Pts',(0.259384667806906,-0.407069005705619,
1.87572597447038));
#10787=CARTESIAN_POINT('Ctrl Pts',(0.295564880870602,-0.411552957311693,
1.87033833905209));
#10788=CARTESIAN_POINT('Ctrl Pts',(0.361953249272518,-0.411552957311693,
1.85863227849762));
#10789=CARTESIAN_POINT('Ctrl Pts',(0.397794208344885,-0.407069005705619,
1.85132063808607));
#10790=CARTESIAN_POINT('Ctrl Pts',(0.466372387779211,-0.388075792674377,
1.83524525067264));
#10791=CARTESIAN_POINT('Ctrl Pts',(0.499115122365417,-0.373566122196588,
1.82650552029421));
#10792=CARTESIAN_POINT('Ctrl Pts',(0.55627784773835,-0.339063173951852,
1.8099349185301));
#10793=CARTESIAN_POINT('Ctrl Pts',(0.583568715090836,-0.317173992396757,
1.80124488173997));
#10794=CARTESIAN_POINT('Ctrl Pts',(0.631771046764577,-0.266247928944116,
1.78490921718958));
#10795=CARTESIAN_POINT('Ctrl Pts',(0.652689698303665,-0.237213819614884,
1.77727615696148));
#10796=CARTESIAN_POINT('Ctrl Pts',(0.690718471466875,-0.166529565724165,
1.76289713151763));
#10797=CARTESIAN_POINT('Ctrl Pts',(0.705596189518013,-0.123392992551698,
1.75687121212928));
#10798=CARTESIAN_POINT('Ctrl Pts',(0.71358822996475,-0.07938,1.75361906569237));
#10799=CARTESIAN_POINT('Origin',(0.33427274200884,-0.07938,1.8957549245485));
#10800=CARTESIAN_POINT('Origin',(0.,-0.07938,0.));
#10801=CARTESIAN_POINT('',(-0.580564309297537,-0.07938,1.80203581326062));
#10802=CARTESIAN_POINT('Origin',(0.,-0.07938,0.));
#10803=CARTESIAN_POINT('Origin',(-0.962500000000001,-0.07938,1.66709890228504));
#10804=CARTESIAN_POINT('Origin',(-0.962500000000001,0.,1.66709890228504));
#10805=CARTESIAN_POINT('',(-1.27032663816428,-0.07938,1.40380134701254));
#10806=CARTESIAN_POINT('Ctrl Pts',(-1.27032663816428,-0.07938,1.40380134701254));
#10807=CARTESIAN_POINT('Ctrl Pts',(-1.26392887632193,-0.123392992551698,
1.40959080384008));
#10808=CARTESIAN_POINT('Ctrl Pts',(-1.25200938026802,-0.166529565724166,
1.42034179508297));
#10809=CARTESIAN_POINT('Ctrl Pts',(-1.22119193909219,-0.237213819614885,
1.44686026563443));
#10810=CARTESIAN_POINT('Ctrl Pts',(-1.20414549695735,-0.266247928944117,
1.46118759620237));
#10811=CARTESIAN_POINT('Ctrl Pts',(-1.16443724790971,-0.317173992396758,
1.49302426802369));
#10812=CARTESIAN_POINT('Ctrl Pts',(-1.14176438887219,-0.339063173951853,
1.51052425783311));
#10813=CARTESIAN_POINT('Ctrl Pts',(-1.09371647724559,-0.373566122196589,
1.54564633355776));
#10814=CARTESIAN_POINT('Ctrl Pts',(-1.06593753500724,-0.388075792674378,
1.56505766847808));
#10815=CARTESIAN_POINT('Ctrl Pts',(-1.00699323215303,-0.407069005705619,
1.6036187101659));
#10816=CARTESIAN_POINT('Ctrl Pts',(-0.975814475692339,-0.411552957311693,
1.62274773466534));
#10817=CARTESIAN_POINT('Ctrl Pts',(-0.917433524307661,-0.411552957311693,
1.65645399266283));
#10818=CARTESIAN_POINT('Ctrl Pts',(-0.885277924911194,-0.407069005705619,
1.67389107556648));
#10819=CARTESIAN_POINT('Ctrl Pts',(-0.822410931786043,-0.388075792674377,
1.70565781840267));
#10820=CARTESIAN_POINT('Ctrl Pts',(-0.791710751504505,-0.373566122196588,
1.72000942061118));
#10821=CARTESIAN_POINT('Ctrl Pts',(-0.737270185880016,-0.339063173951852,
1.74405909481629));
#10822=CARTESIAN_POINT('Ctrl Pts',(-0.710778320620332,-0.317173992396757,
1.75494437181449));
#10823=CARTESIAN_POINT('Ctrl Pts',(-0.663352829527299,-0.266247928944116,
1.77341438831889));
#10824=CARTESIAN_POINT('Ctrl Pts',(-0.642421776219621,-0.237213819614884,
1.78101337496783));
#10825=CARTESIAN_POINT('Ctrl Pts',(-0.604047386464641,-0.166529565724165,
1.79444282663));
#10826=CARTESIAN_POINT('Ctrl Pts',(-0.588777006905475,-0.123392992551698,
1.79938991739155));
#10827=CARTESIAN_POINT('Ctrl Pts',(-0.580564309297537,-0.0793799999999999,
1.80203581326062));
#10828=CARTESIAN_POINT('Origin',(-0.962500000000001,-0.07938,1.66709890228504));
#10829=CARTESIAN_POINT('Origin',(0.,-0.07938,0.));
#10830=CARTESIAN_POINT('',(-1.60306435598592,-0.07938,1.00725997640701));
#10831=CARTESIAN_POINT('Origin',(0.,-0.07938,0.));
#10832=CARTESIAN_POINT('Origin',(-1.80890829501287,-0.07938,0.658388775901912));
#10833=CARTESIAN_POINT('Origin',(-1.80890829501287,0.,0.658388775901912));
#10834=CARTESIAN_POINT('',(-1.8754727744327,-0.07938,0.258823997855139));
#10835=CARTESIAN_POINT('Ctrl Pts',(-1.8754727744327,-0.07938,0.258823997855138));
#10836=CARTESIAN_POINT('Ctrl Pts',(-1.87429319564052,-0.123392992551698,
0.267371381128541));
#10837=CARTESIAN_POINT('Ctrl Pts',(-1.87207293588642,-0.166529565724165,
0.283268822605344));
#10838=CARTESIAN_POINT('Ctrl Pts',(-1.86551115062085,-0.237213819614884,
0.323392218961362));
#10839=CARTESIAN_POINT('Ctrl Pts',(-1.86166224891746,-0.266247928944116,
0.34532483272118));
#10840=CARTESIAN_POINT('Ctrl Pts',(-1.85170818356893,-0.317173992396757,
0.395237108747477));
#10841=CARTESIAN_POINT('Ctrl Pts',(-1.84558854251276,-0.339063173951852,
0.423216711561106));
#10842=CARTESIAN_POINT('Ctrl Pts',(-1.83135774191,-0.373566122196588,0.481006384765672));
#10843=CARTESIAN_POINT('Ctrl Pts',(-1.82255520314685,-0.388075792674377,
0.513732289895913));
#10844=CARTESIAN_POINT('Ctrl Pts',(-1.8021878073054,-0.407069005705619,
0.581160429138046));
#10845=CARTESIAN_POINT('Ctrl Pts',(-1.79059939410895,-0.411552957311693,
0.615855430396488));
#10846=CARTESIAN_POINT('Ctrl Pts',(-1.76754295572641,-0.411552957311693,
0.679202474225583));
#10847=CARTESIAN_POINT('Ctrl Pts',(-1.75411867833313,-0.407069005705619,
0.713229275562222));
#10848=CARTESIAN_POINT('Ctrl Pts',(-1.72637903628921,-0.388075792674378,
0.777974136626975));
#10849=CARTESIAN_POINT('Ctrl Pts',(-1.71208636586057,-0.373566122196588,
0.808701797248777));
#10850=CARTESIAN_POINT('Ctrl Pts',(-1.68584130567972,-0.339063173951852,
0.862118637580169));
#10851=CARTESIAN_POINT('Ctrl Pts',(-1.67254428069212,-0.317173992396757,
0.88748588628286));
#10852=CARTESIAN_POINT('Ctrl Pts',(-1.64808654453785,-0.266247928944116,
0.932119257848273));
#10853=CARTESIAN_POINT('Ctrl Pts',(-1.63693696192699,-0.237213819614884,
0.951394641067894));
#10854=CARTESIAN_POINT('Ctrl Pts',(-1.61617275903043,-0.166529565724165,
0.986348780151617));
#10855=CARTESIAN_POINT('Ctrl Pts',(-1.60765489827034,-0.123392992551698,
0.999954082314951));
#10856=CARTESIAN_POINT('Ctrl Pts',(-1.60306435598592,-0.07938,1.00725997640701));
#10857=CARTESIAN_POINT('Origin',(-1.80890829501287,-0.07938,0.658388775901912));
#10858=CARTESIAN_POINT('Origin',(0.,-0.07938,0.));
#10859=CARTESIAN_POINT('',(-1.893248,-0.0793799999999999,2.31856010319213E-16));
#10860=CARTESIAN_POINT('Origin',(0.,-0.07938,0.));
#10861=CARTESIAN_POINT('',(-1.8754727744327,-0.07938,-0.258823997855139));
#10862=CARTESIAN_POINT('Origin',(0.,-0.07938,0.));
#10863=CARTESIAN_POINT('Origin',(-1.80890829501287,-0.07938,-0.658388775901913));
#10864=CARTESIAN_POINT('Origin',(-1.80890829501287,0.,-0.658388775901913));
#10865=CARTESIAN_POINT('',(-1.60306435598592,-0.07938,-1.00725997640701));
#10866=CARTESIAN_POINT('Ctrl Pts',(-1.60306435598592,-0.07938,-1.00725997640701));
#10867=CARTESIAN_POINT('Ctrl Pts',(-1.60765489827034,-0.123392992551698,
-0.999954082314952));
#10868=CARTESIAN_POINT('Ctrl Pts',(-1.61617275903043,-0.166529565724166,
-0.986348780151617));
#10869=CARTESIAN_POINT('Ctrl Pts',(-1.63693696192699,-0.237213819614884,
-0.951394641067894));
#10870=CARTESIAN_POINT('Ctrl Pts',(-1.64808654453785,-0.266247928944116,
-0.932119257848273));
#10871=CARTESIAN_POINT('Ctrl Pts',(-1.67254428069212,-0.317173992396757,
-0.88748588628286));
#10872=CARTESIAN_POINT('Ctrl Pts',(-1.68584130567972,-0.339063173951852,
-0.862118637580169));
#10873=CARTESIAN_POINT('Ctrl Pts',(-1.71208636586057,-0.373566122196588,
-0.808701797248777));
#10874=CARTESIAN_POINT('Ctrl Pts',(-1.72637903628921,-0.388075792674377,
-0.777974136626975));
#10875=CARTESIAN_POINT('Ctrl Pts',(-1.75411867833313,-0.407069005705619,
-0.713229275562223));
#10876=CARTESIAN_POINT('Ctrl Pts',(-1.76754295572641,-0.411552957311693,
-0.679202474225584));
#10877=CARTESIAN_POINT('Ctrl Pts',(-1.79059939410895,-0.411552957311693,
-0.615855430396488));
#10878=CARTESIAN_POINT('Ctrl Pts',(-1.8021878073054,-0.407069005705619,
-0.581160429138047));
#10879=CARTESIAN_POINT('Ctrl Pts',(-1.82255520314685,-0.388075792674378,
-0.513732289895914));
#10880=CARTESIAN_POINT('Ctrl Pts',(-1.83135774191,-0.373566122196588,-0.481006384765673));
#10881=CARTESIAN_POINT('Ctrl Pts',(-1.84558854251276,-0.339063173951852,
-0.423216711561107));
#10882=CARTESIAN_POINT('Ctrl Pts',(-1.85170818356893,-0.317173992396757,
-0.395237108747477));
#10883=CARTESIAN_POINT('Ctrl Pts',(-1.86166224891746,-0.266247928944116,
-0.34532483272118));
#10884=CARTESIAN_POINT('Ctrl Pts',(-1.86551115062085,-0.237213819614884,
-0.323392218961362));
#10885=CARTESIAN_POINT('Ctrl Pts',(-1.87207293588642,-0.166529565724166,
-0.283268822605344));
#10886=CARTESIAN_POINT('Ctrl Pts',(-1.87429319564052,-0.123392992551698,
-0.267371381128542));
#10887=CARTESIAN_POINT('Ctrl Pts',(-1.8754727744327,-0.07938,-0.258823997855139));
#10888=CARTESIAN_POINT('Origin',(-1.80890829501287,-0.07938,-0.658388775901913));
#10889=CARTESIAN_POINT('Origin',(0.,-0.07938,0.));
#10890=CARTESIAN_POINT('',(-1.27032663816428,-0.07938,-1.40380134701254));
#10891=CARTESIAN_POINT('Origin',(0.,-0.07938,0.));
#10892=CARTESIAN_POINT('Origin',(-0.9625,-0.07938,-1.66709890228504));
#10893=CARTESIAN_POINT('Origin',(-0.9625,0.,-1.66709890228504));
#10894=CARTESIAN_POINT('',(-0.580564309297535,-0.07938,-1.80203581326062));
#10895=CARTESIAN_POINT('Ctrl Pts',(-0.580564309297535,-0.07938,-1.80203581326062));
#10896=CARTESIAN_POINT('Ctrl Pts',(-0.588777006905474,-0.123392992551698,
-1.79938991739155));
#10897=CARTESIAN_POINT('Ctrl Pts',(-0.60404738646464,-0.166529565724165,
-1.79444282663));
#10898=CARTESIAN_POINT('Ctrl Pts',(-0.642421776219619,-0.237213819614884,
-1.78101337496783));
#10899=CARTESIAN_POINT('Ctrl Pts',(-0.663352829527298,-0.266247928944116,
-1.77341438831889));
#10900=CARTESIAN_POINT('Ctrl Pts',(-0.71077832062033,-0.317173992396757,
-1.75494437181449));
#10901=CARTESIAN_POINT('Ctrl Pts',(-0.737270185880015,-0.339063173951852,
-1.74405909481629));
#10902=CARTESIAN_POINT('Ctrl Pts',(-0.791710751504504,-0.373566122196588,
-1.72000942061118));
#10903=CARTESIAN_POINT('Ctrl Pts',(-0.822410931786042,-0.388075792674378,
-1.70565781840267));
#10904=CARTESIAN_POINT('Ctrl Pts',(-0.885277924911194,-0.407069005705619,
-1.67389107556648));
#10905=CARTESIAN_POINT('Ctrl Pts',(-0.917433524307661,-0.411552957311693,
-1.65645399266283));
#10906=CARTESIAN_POINT('Ctrl Pts',(-0.975814475692338,-0.411552957311693,
-1.62274773466534));
#10907=CARTESIAN_POINT('Ctrl Pts',(-1.00699323215303,-0.407069005705619,
-1.60361871016591));
#10908=CARTESIAN_POINT('Ctrl Pts',(-1.06593753500724,-0.388075792674378,
-1.56505766847808));
#10909=CARTESIAN_POINT('Ctrl Pts',(-1.09371647724559,-0.373566122196588,
-1.54564633355776));
#10910=CARTESIAN_POINT('Ctrl Pts',(-1.14176438887219,-0.339063173951852,
-1.51052425783311));
#10911=CARTESIAN_POINT('Ctrl Pts',(-1.1644372479097,-0.317173992396757,
-1.49302426802369));
#10912=CARTESIAN_POINT('Ctrl Pts',(-1.20414549695735,-0.266247928944116,
-1.46118759620237));
#10913=CARTESIAN_POINT('Ctrl Pts',(-1.22119193909219,-0.237213819614884,
-1.44686026563443));
#10914=CARTESIAN_POINT('Ctrl Pts',(-1.25200938026802,-0.166529565724166,
-1.42034179508298));
#10915=CARTESIAN_POINT('Ctrl Pts',(-1.26392887632193,-0.123392992551698,
-1.40959080384008));
#10916=CARTESIAN_POINT('Ctrl Pts',(-1.27032663816428,-0.07938,-1.40380134701254));
#10917=CARTESIAN_POINT('Origin',(-0.9625,-0.07938,-1.66709890228504));
#10918=CARTESIAN_POINT('Origin',(0.,-0.07938,0.));
#10919=CARTESIAN_POINT('',(-0.0707805497908242,-0.07938,-1.89192444438865));
#10920=CARTESIAN_POINT('Origin',(0.,-0.07938,0.));
#10921=CARTESIAN_POINT('Origin',(0.334272742008841,-0.07938,-1.8957549245485));
#10922=CARTESIAN_POINT('Origin',(0.334272742008841,0.,-1.8957549245485));
#10923=CARTESIAN_POINT('',(0.71358822996475,-0.07938,-1.75361906569237));
#10924=CARTESIAN_POINT('Ctrl Pts',(0.71358822996475,-0.07938,-1.75361906569237));
#10925=CARTESIAN_POINT('Ctrl Pts',(0.705596189518014,-0.123392992551698,
-1.75687121212928));
#10926=CARTESIAN_POINT('Ctrl Pts',(0.690718471466876,-0.166529565724166,
-1.76289713151763));
#10927=CARTESIAN_POINT('Ctrl Pts',(0.652689698303666,-0.237213819614884,
-1.77727615696148));
#10928=CARTESIAN_POINT('Ctrl Pts',(0.631771046764578,-0.266247928944116,
-1.78490921718958));
#10929=CARTESIAN_POINT('Ctrl Pts',(0.583568715090837,-0.317173992396757,
-1.80124488173997));
#10930=CARTESIAN_POINT('Ctrl Pts',(0.556277847738351,-0.339063173951852,
-1.8099349185301));
#10931=CARTESIAN_POINT('Ctrl Pts',(0.499115122365417,-0.373566122196588,
-1.8265055202942));
#10932=CARTESIAN_POINT('Ctrl Pts',(0.466372387779211,-0.388075792674378,
-1.83524525067263));
#10933=CARTESIAN_POINT('Ctrl Pts',(0.397794208344886,-0.407069005705619,
-1.85132063808607));
#10934=CARTESIAN_POINT('Ctrl Pts',(0.361953249272519,-0.411552957311693,
-1.85863227849762));
#10935=CARTESIAN_POINT('Ctrl Pts',(0.295564880870602,-0.411552957311693,
-1.87033833905209));
#10936=CARTESIAN_POINT('Ctrl Pts',(0.259384667806906,-0.407069005705619,
-1.87572597447038));
#10937=CARTESIAN_POINT('Ctrl Pts',(0.189444152338379,-0.388075792674377,
-1.88407517030084));
#10938=CARTESIAN_POINT('Ctrl Pts',(0.155686882426711,-0.373566122196588,
-1.88706118493262));
#10939=CARTESIAN_POINT('Ctrl Pts',(0.096304011619402,-0.339063173951852,
-1.89104071625784));
#10940=CARTESIAN_POINT('Ctrl Pts',(0.0676868173249583,-0.317173992396757,
-1.89220877917518));
#10941=CARTESIAN_POINT('Ctrl Pts',(0.0168043156156251,-0.266247928944116,
-1.89334444412923));
#10942=CARTESIAN_POINT('Ctrl Pts',(-0.00546344722567807,-0.237213819614884,
-1.89332631395644));
#10943=CARTESIAN_POINT('Ctrl Pts',(-0.0461167210878748,-0.166529565724165,
-1.89282105630055));
#10944=CARTESIAN_POINT('Ctrl Pts',(-0.0621581887675344,-0.123392992551698,
-1.89224702357808));
#10945=CARTESIAN_POINT('Ctrl Pts',(-0.0707805497908242,-0.07938,-1.89192444438865));
#10946=CARTESIAN_POINT('Origin',(0.334272742008841,-0.07938,-1.8957549245485));
#10947=CARTESIAN_POINT('Origin',(0.,-0.07938,0.));
#10948=CARTESIAN_POINT('',(1.16188454446795,-0.07938,-1.49479506783723));
#10949=CARTESIAN_POINT('Origin',(0.,-0.07938,0.));
#10950=CARTESIAN_POINT('Origin',(1.47463555300403,-0.07938,-1.23736614864659));
#10951=CARTESIAN_POINT('Origin',(1.47463555300403,0.,-1.23736614864659));
#10952=CARTESIAN_POINT('',(1.67384490577674,-0.07938,-0.884664467981643));
#10953=CARTESIAN_POINT('Ctrl Pts',(1.67384490577674,-0.07938,-0.884664467981643));
#10954=CARTESIAN_POINT('Ctrl Pts',(1.66981308703787,-0.123392992551698,
-0.892292941263125));
#10955=CARTESIAN_POINT('Ctrl Pts',(1.66228948011831,-0.166529565724165,
-0.906472276148934));
#10956=CARTESIAN_POINT('Ctrl Pts',(1.64240040915267,-0.237213819614884,
-0.941931672888549));
#10957=CARTESIAN_POINT('Ctrl Pts',(1.63128222892223,-0.266247928944116,
-0.961225186280958));
#10958=CARTESIAN_POINT('Ctrl Pts',(1.60485746336717,-0.317173992396757,
-1.00472289289232));
#10959=CARTESIAN_POINT('Ctrl Pts',(1.58953729406031,-0.339063173951852,
-1.02892207867768));
#10960=CARTESIAN_POINT('Ctrl Pts',(1.55639948343386,-0.373566122196588,
-1.07835938768384));
#10961=CARTESIAN_POINT('Ctrl Pts',(1.53693488395083,-0.388075792674377,
-1.10610103367386));
#10962=CARTESIAN_POINT('Ctrl Pts',(1.49473401052622,-0.407069005705619,
-1.16249669890816));
#10963=CARTESIAN_POINT('Ctrl Pts',(1.4719780748558,-0.411552957311693,-1.19113586482651));
#10964=CARTESIAN_POINT('Ctrl Pts',(1.42864614483643,-0.411552957311693,
-1.24277684810113));
#10965=CARTESIAN_POINT('Ctrl Pts',(1.40439359896051,-0.407069005705619,
-1.27016020894803));
#10966=CARTESIAN_POINT('Ctrl Pts',(1.35618281536764,-0.388075792674378,
-1.32151296077672));
#10967=CARTESIAN_POINT('Ctrl Pts',(1.33224261954459,-0.373566122196588,
-1.34549913552853));
#10968=CARTESIAN_POINT('Ctrl Pts',(1.28931069477441,-0.339063173951852,
-1.38671820696899));
#10969=CARTESIAN_POINT('Ctrl Pts',(1.26813946847809,-0.317173992396757,
-1.40600777299249));
#10970=CARTESIAN_POINT('Ctrl Pts',(1.22989120215289,-0.266247928944116,
-1.4395843844684));
#10971=CARTESIAN_POINT('Ctrl Pts',(1.21282145231718,-0.237213819614884,
-1.45388393800011));
#10972=CARTESIAN_POINT('Ctrl Pts',(1.18135446441955,-0.166529565724166,
-1.47962830891229));
#10973=CARTESIAN_POINT('Ctrl Pts',(1.16869700612251,-0.123392992551698,
-1.48949983100074));
#10974=CARTESIAN_POINT('Ctrl Pts',(1.16188454446795,-0.0793799999999999,
-1.49479506783723));
#10975=CARTESIAN_POINT('Origin',(1.47463555300403,-0.07938,-1.23736614864659));
#10976=CARTESIAN_POINT('Origin',(0.,-0.27783,0.));
#10977=CARTESIAN_POINT('',(-1.893248,-0.47628,2.31856010319213E-16));
#10978=CARTESIAN_POINT('Origin',(0.,-0.47628,0.));
#10979=CARTESIAN_POINT('',(-1.893248,-0.27783,2.31856010319213E-16));
#10980=CARTESIAN_POINT('',(1.85089094746182,-0.07938,0.39823446624808));
#10981=CARTESIAN_POINT('Origin',(0.,-0.07938,0.));
#10982=CARTESIAN_POINT('',(1.85089094746182,-0.07938,-0.39823446624808));
#10983=CARTESIAN_POINT('Ctrl Pts',(1.85089094746182,-0.07938,0.39823446624808));
#10984=CARTESIAN_POINT('Ctrl Pts',(1.8527058832274,-0.123392992551698,0.38979911355147));
#10985=CARTESIAN_POINT('Ctrl Pts',(1.85605676673266,-0.166529565724166,
0.374101031547026));
#10986=CARTESIAN_POINT('Ctrl Pts',(1.86361371531181,-0.237213819614884,
0.334153109333404));
#10987=CARTESIAN_POINT('Ctrl Pts',(1.86749832648465,-0.266247928944116,
0.312226792116516));
#10988=CARTESIAN_POINT('Ctrl Pts',(1.87521556853004,-0.317173992396757,
0.261920103790797));
#10989=CARTESIAN_POINT('Ctrl Pts',(1.87903457475221,-0.339063173951852,
0.233534836983177));
#10990=CARTESIAN_POINT('Ctrl Pts',(1.88542722875009,-0.373566122196588,
0.174363087053423));
#10991=CARTESIAN_POINT('Ctrl Pts',(1.88834846679328,-0.388075792674378,
0.140600149924591));
#10992=CARTESIAN_POINT('Ctrl Pts',(1.89227115706422,-0.407069005705619,
0.0702723654005715));
#10993=CARTESIAN_POINT('Ctrl Pts',(1.893248,-0.411552957311693,0.0337062579974903));
#10994=CARTESIAN_POINT('Ctrl Pts',(1.893248,-0.411552957311693,-0.0337062579974903));
#10995=CARTESIAN_POINT('Ctrl Pts',(1.89227115706422,-0.407069005705619,
-0.0702723654005715));
#10996=CARTESIAN_POINT('Ctrl Pts',(1.88834846679328,-0.388075792674378,
-0.140600149924591));
#10997=CARTESIAN_POINT('Ctrl Pts',(1.88542722875009,-0.373566122196588,
-0.174363087053422));
#10998=CARTESIAN_POINT('Ctrl Pts',(1.87903457475221,-0.339063173951852,
-0.233534836983177));
#10999=CARTESIAN_POINT('Ctrl Pts',(1.87521556853004,-0.317173992396757,
-0.261920103790797));
#11000=CARTESIAN_POINT('Ctrl Pts',(1.86749832648465,-0.266247928944116,
-0.312226792116516));
#11001=CARTESIAN_POINT('Ctrl Pts',(1.86361371531181,-0.237213819614884,
-0.334153109333404));
#11002=CARTESIAN_POINT('Ctrl Pts',(1.85605676673266,-0.166529565724166,
-0.374101031547026));
#11003=CARTESIAN_POINT('Ctrl Pts',(1.8527058832274,-0.123392992551698,-0.38979911355147));
#11004=CARTESIAN_POINT('Ctrl Pts',(1.85089094746182,-0.07938,-0.39823446624808));
#11005=CARTESIAN_POINT('Origin',(0.,-0.07938,0.));
#11006=CARTESIAN_POINT('Origin',(0.,-0.07938,0.));
#11007=CARTESIAN_POINT('Origin',(1.925,-0.07938,0.));
#11008=CARTESIAN_POINT('Origin',(1.925,0.,0.));
#11009=CARTESIAN_POINT('Origin',(1.925,-0.07938,0.));
#11010=CARTESIAN_POINT('Origin',(0.,-0.47628,0.));
#11011=CARTESIAN_POINT('Origin',(0.,-0.07938,0.));
#11012=CARTESIAN_POINT('',(0.,0.,0.));
#11013=CARTESIAN_POINT('Origin',(1.95469,0.745,0.));
#11014=CARTESIAN_POINT('',(-1.95469,0.745,-2.39380485182534E-16));
#11015=CARTESIAN_POINT('Origin',(0.,0.745,0.));
#11016=CARTESIAN_POINT('',(-1.90031,0.745,-2.32720855888771E-16));
#11017=CARTESIAN_POINT('Origin',(0.,0.745,0.));
#11018=CARTESIAN_POINT('Origin',(0.,0.7075,0.));
#11019=CARTESIAN_POINT('',(-1.95469,0.67,-2.39380485182534E-16));
#11020=CARTESIAN_POINT('Origin',(0.,0.67,0.));
#11021=CARTESIAN_POINT('',(-1.95469,0.7075,-2.39380485182534E-16));
#11022=CARTESIAN_POINT('Origin',(1.90031,0.67,0.));
#11023=CARTESIAN_POINT('',(-1.90031,0.67,-2.32720855888771E-16));
#11024=CARTESIAN_POINT('Origin',(0.,0.67,0.));
#11025=CARTESIAN_POINT('Origin',(0.,0.7075,0.));
#11026=CARTESIAN_POINT('',(-1.90031,0.7075,-2.32720855888771E-16));
#11027=CARTESIAN_POINT('Origin',(1.95469,-0.67,0.));
#11028=CARTESIAN_POINT('',(-1.95469,-0.67,-2.39380485182534E-16));
#11029=CARTESIAN_POINT('Origin',(0.,-0.67,0.));
#11030=CARTESIAN_POINT('',(-1.90031,-0.67,-2.32720855888771E-16));
#11031=CARTESIAN_POINT('Origin',(0.,-0.67,0.));
#11032=CARTESIAN_POINT('Origin',(0.,-0.7075,0.));
#11033=CARTESIAN_POINT('',(-1.95469,-0.745,-2.39380485182534E-16));
#11034=CARTESIAN_POINT('Origin',(0.,-0.745,0.));
#11035=CARTESIAN_POINT('',(-1.95469,-0.7075,-2.39380485182534E-16));
#11036=CARTESIAN_POINT('Origin',(1.90031,-0.745,0.));
#11037=CARTESIAN_POINT('',(-1.90031,-0.745,-2.32720855888771E-16));
#11038=CARTESIAN_POINT('Origin',(0.,-0.745,0.));
#11039=CARTESIAN_POINT('Origin',(0.,-0.7075,0.));
#11040=CARTESIAN_POINT('',(-1.90031,-0.7075,-2.32720855888771E-16));
#11041=CARTESIAN_POINT('',(0.,0.,0.));
#11042=CARTESIAN_POINT('',(0.,0.,0.));
#11043=CARTESIAN_POINT('',(0.,0.,0.));
#11044=CARTESIAN_POINT('',(0.,0.,0.));
#11045=CARTESIAN_POINT('',(0.,0.,0.));
#11046=CARTESIAN_POINT('',(0.,0.,0.));
#11047=CARTESIAN_POINT('Origin',(0.45,0.6,0.));
#11048=CARTESIAN_POINT('',(-0.45,0.6,-5.51091059616309E-17));
#11049=CARTESIAN_POINT('Origin',(0.,0.6,0.));
#11050=CARTESIAN_POINT('Origin',(0.,0.575,0.));
#11051=CARTESIAN_POINT('',(-0.5,0.55,-6.12323399573677E-17));
#11052=CARTESIAN_POINT('Origin',(0.,0.55,0.));
#11053=CARTESIAN_POINT('',(-0.475,0.575,-5.81707229594993E-17));
#11054=CARTESIAN_POINT('Origin',(0.,0.29,0.));
#11055=CARTESIAN_POINT('',(-0.5,0.0299999999999998,-6.12323399573677E-17));
#11056=CARTESIAN_POINT('Origin',(0.,0.0299999999999998,0.));
#11057=CARTESIAN_POINT('',(-0.5,0.29,-6.12323399573677E-17));
#11058=CARTESIAN_POINT('Origin',(0.,0.0150000000000001,0.));
#11059=CARTESIAN_POINT('',(-0.47,7.11236625150491E-17,-5.75583995599256E-17));
#11060=CARTESIAN_POINT('Origin',(0.,0.,0.));
#11061=CARTESIAN_POINT('',(-0.485,0.0150000000000001,-5.93953697586466E-17));
#11062=CARTESIAN_POINT('Origin',(0.32,0.,0.));
#11063=CARTESIAN_POINT('',(-0.32,-6.93889390390723E-18,-3.91886975727153E-17));
#11064=CARTESIAN_POINT('Origin',(0.,0.,0.));
#11065=CARTESIAN_POINT('Origin',(0.,-0.02,0.));
#11066=CARTESIAN_POINT('',(-0.2942,-0.0515999999999999,3.60291088309151E-17));
#11067=CARTESIAN_POINT('Origin',(0.,-0.0515999999999999,0.));
#11068=CARTESIAN_POINT('',(-0.31,-0.02,-3.7964050773568E-17));
#11069=CARTESIAN_POINT('Origin',(0.,-1.24,0.));
#11070=CARTESIAN_POINT('',(-0.2942,-2.4458,3.60291088309151E-17));
#11071=CARTESIAN_POINT('Origin',(0.,-2.4458,0.));
#11072=CARTESIAN_POINT('',(-0.2942,-1.24,-3.60291088309151E-17));
#11073=CARTESIAN_POINT('Origin',(0.,-2.47,0.));
#11074=CARTESIAN_POINT('',(-0.24,-2.5,-2.93915231795365E-17));
#11075=CARTESIAN_POINT('Origin',(0.,-2.5,0.));
#11076=CARTESIAN_POINT('',(-0.27,-2.47,-3.30654635769785E-17));
#11077=CARTESIAN_POINT('Origin',(0.,-2.5,0.));
#11078=CARTESIAN_POINT('Origin',(0.144337567297406,-0.6,-0.25));
#11079=CARTESIAN_POINT('',(0.288675134594813,-0.6,0.));
#11080=CARTESIAN_POINT('',(0.144337567297406,-0.6,-0.25));
#11081=CARTESIAN_POINT('',(0.288675134594813,-0.6,0.));
#11082=CARTESIAN_POINT('',(0.144337567297406,-0.96,-0.25));
#11083=CARTESIAN_POINT('',(0.144337567297406,-0.6,-0.25));
#11084=CARTESIAN_POINT('',(0.288675134594813,-0.96,0.));
#11085=CARTESIAN_POINT('',(0.288675134594813,-0.96,0.));
#11086=CARTESIAN_POINT('',(0.288675134594813,-0.6,0.));
#11087=CARTESIAN_POINT('Origin',(-0.144337567297406,-0.6,-0.25));
#11088=CARTESIAN_POINT('',(-0.144337567297406,-0.6,-0.25));
#11089=CARTESIAN_POINT('',(0.144337567297406,-0.6,-0.25));
#11090=CARTESIAN_POINT('',(-0.144337567297406,-0.96,-0.25));
#11091=CARTESIAN_POINT('',(-0.144337567297406,-0.6,-0.25));
#11092=CARTESIAN_POINT('',(0.144337567297406,-0.96,-0.25));
#11093=CARTESIAN_POINT('Origin',(-0.288675134594813,-0.6,-8.32667268468867E-17));
#11094=CARTESIAN_POINT('',(-0.288675134594813,-0.6,-3.53525079574969E-17));
#11095=CARTESIAN_POINT('',(-0.144337567297406,-0.6,-0.25));
#11096=CARTESIAN_POINT('',(-0.288675134594813,-0.96,-5.55111512312578E-17));
#11097=CARTESIAN_POINT('',(-0.288675134594813,-0.6,-3.53525079574969E-17));
#11098=CARTESIAN_POINT('',(-0.144337567297406,-0.96,-0.25));
#11099=CARTESIAN_POINT('Origin',(-0.144337567297407,-0.6,0.25));
#11100=CARTESIAN_POINT('',(-0.144337567297407,-0.6,0.25));
#11101=CARTESIAN_POINT('',(-0.288675134594813,-0.6,-3.53525079574969E-17));
#11102=CARTESIAN_POINT('',(-0.144337567297407,-0.96,0.25));
#11103=CARTESIAN_POINT('',(-0.144337567297407,-0.6,0.25));
#11104=CARTESIAN_POINT('',(-0.288675134594813,-0.96,-3.53525079574969E-17));
#11105=CARTESIAN_POINT('Origin',(0.144337567297406,-0.6,0.25));
#11106=CARTESIAN_POINT('',(0.144337567297406,-0.6,0.25));
#11107=CARTESIAN_POINT('',(-0.144337567297407,-0.6,0.25));
#11108=CARTESIAN_POINT('',(0.144337567297406,-0.96,0.25));
#11109=CARTESIAN_POINT('',(0.144337567297406,-0.6,0.25));
#11110=CARTESIAN_POINT('',(-0.144337567297407,-0.96,0.25));
#11111=CARTESIAN_POINT('Origin',(0.288675134594813,-0.6,0.));
#11112=CARTESIAN_POINT('',(0.144337567297406,-0.6,0.25));
#11113=CARTESIAN_POINT('',(0.144337567297406,-0.96,0.25));
#11114=CARTESIAN_POINT('Origin',(0.,-0.6,0.));
#11115=CARTESIAN_POINT('Origin',(0.,-0.96,0.));
#11116=CARTESIAN_POINT('',(0.,0.,0.));
#11117=CARTESIAN_POINT('Origin',(0.3,0.4,0.));
#11118=CARTESIAN_POINT('',(-0.3,0.4,-3.67394039744206E-17));
#11119=CARTESIAN_POINT('Origin',(0.,0.4,0.));
#11120=CARTESIAN_POINT('Origin',(0.,0.375,0.));
#11121=CARTESIAN_POINT('',(-0.35,0.35,-4.28626379701573E-17));
#11122=CARTESIAN_POINT('Origin',(0.,0.35,0.));
#11123=CARTESIAN_POINT('',(-0.325,0.375,-3.9801020972289E-17));
#11124=CARTESIAN_POINT('Origin',(0.,0.19,0.));
#11125=CARTESIAN_POINT('',(-0.35,0.03,-4.28626379701574E-17));
#11126=CARTESIAN_POINT('Origin',(0.,0.03,0.));
#11127=CARTESIAN_POINT('',(-0.35,0.19,-4.28626379701574E-17));
#11128=CARTESIAN_POINT('Origin',(0.,0.0149999999999999,0.));
#11129=CARTESIAN_POINT('',(-0.32,-3.29597460435593E-17,-3.91886975727153E-17));
#11130=CARTESIAN_POINT('Origin',(0.,0.,0.));
#11131=CARTESIAN_POINT('',(-0.335,0.0149999999999999,-4.10256677714363E-17));
#11132=CARTESIAN_POINT('Origin',(0.22,0.,0.));
#11133=CARTESIAN_POINT('',(-0.22,-6.93889390390723E-18,-2.69422295812418E-17));
#11134=CARTESIAN_POINT('Origin',(0.,0.,0.));
#11135=CARTESIAN_POINT('Origin',(0.,-0.02,0.));
#11136=CARTESIAN_POINT('',(-0.1954,-0.0492,2.39295984553393E-17));
#11137=CARTESIAN_POINT('Origin',(0.,-0.0492,0.));
#11138=CARTESIAN_POINT('',(-0.21,-0.02,-2.57175827820944E-17));
#11139=CARTESIAN_POINT('Origin',(0.,-0.8,0.));
#11140=CARTESIAN_POINT('',(-0.1954,-1.5646,2.39295984553393E-17));
#11141=CARTESIAN_POINT('Origin',(0.,-1.5646,0.));
#11142=CARTESIAN_POINT('',(-0.1954,-0.8,-2.39295984553393E-17));
#11143=CARTESIAN_POINT('Origin',(0.,-1.58,0.));
#11144=CARTESIAN_POINT('',(-0.16,-1.6,-1.95943487863577E-17));
#11145=CARTESIAN_POINT('Origin',(0.,-1.6,0.));
#11146=CARTESIAN_POINT('',(-0.18,-1.58,-2.20436423846524E-17));
#11147=CARTESIAN_POINT('Origin',(0.,-1.6,0.));
#11148=CARTESIAN_POINT('Origin',(0.0866025403784439,-0.4,-0.15));
#11149=CARTESIAN_POINT('',(0.173205080756888,-0.4,0.));
#11150=CARTESIAN_POINT('',(0.0866025403784439,-0.4,-0.15));
#11151=CARTESIAN_POINT('',(0.173205080756888,-0.4,0.));
#11152=CARTESIAN_POINT('',(0.0866025403784439,-0.64,-0.15));
#11153=CARTESIAN_POINT('',(0.0866025403784439,-0.4,-0.15));
#11154=CARTESIAN_POINT('',(0.173205080756888,-0.64,0.));
#11155=CARTESIAN_POINT('',(0.173205080756888,-0.64,0.));
#11156=CARTESIAN_POINT('',(0.173205080756888,-0.4,0.));
#11157=CARTESIAN_POINT('Origin',(-0.0866025403784438,-0.4,-0.15));
#11158=CARTESIAN_POINT('',(-0.0866025403784438,-0.4,-0.15));
#11159=CARTESIAN_POINT('',(0.0866025403784439,-0.4,-0.15));
#11160=CARTESIAN_POINT('',(-0.0866025403784438,-0.64,-0.15));
#11161=CARTESIAN_POINT('',(-0.0866025403784438,-0.4,-0.15));
#11162=CARTESIAN_POINT('',(0.0866025403784439,-0.64,-0.15));
#11163=CARTESIAN_POINT('Origin',(-0.173205080756888,-0.4,-2.77555756156289E-17));
#11164=CARTESIAN_POINT('',(-0.173205080756888,-0.4,-2.12115047744981E-17));
#11165=CARTESIAN_POINT('',(-0.0866025403784438,-0.4,-0.15));
#11166=CARTESIAN_POINT('',(-0.173205080756888,-0.64,-2.77555756156289E-17));
#11167=CARTESIAN_POINT('',(-0.173205080756888,-0.4,-2.12115047744981E-17));
#11168=CARTESIAN_POINT('',(-0.0866025403784438,-0.64,-0.15));
#11169=CARTESIAN_POINT('Origin',(-0.0866025403784439,-0.4,0.15));
#11170=CARTESIAN_POINT('',(-0.0866025403784439,-0.4,0.15));
#11171=CARTESIAN_POINT('',(-0.173205080756888,-0.4,-2.12115047744981E-17));
#11172=CARTESIAN_POINT('',(-0.0866025403784439,-0.64,0.15));
#11173=CARTESIAN_POINT('',(-0.0866025403784439,-0.4,0.15));
#11174=CARTESIAN_POINT('',(-0.173205080756888,-0.64,-2.12115047744981E-17));
#11175=CARTESIAN_POINT('Origin',(0.0866025403784439,-0.4,0.15));
#11176=CARTESIAN_POINT('',(0.0866025403784439,-0.4,0.15));
#11177=CARTESIAN_POINT('',(-0.0866025403784439,-0.4,0.15));
#11178=CARTESIAN_POINT('',(0.0866025403784439,-0.64,0.15));
#11179=CARTESIAN_POINT('',(0.0866025403784439,-0.4,0.15));
#11180=CARTESIAN_POINT('',(-0.0866025403784439,-0.64,0.15));
#11181=CARTESIAN_POINT('Origin',(0.173205080756888,-0.4,0.));
#11182=CARTESIAN_POINT('',(0.0866025403784439,-0.4,0.15));
#11183=CARTESIAN_POINT('',(0.0866025403784439,-0.64,0.15));
#11184=CARTESIAN_POINT('Origin',(0.,-0.4,-2.77555756156289E-17));
#11185=CARTESIAN_POINT('Origin',(0.,-0.64,-2.77555756156289E-17));
#11186=CARTESIAN_POINT('',(0.,0.,0.));
#11187=CARTESIAN_POINT('',(0.,0.,0.));
#11188=CARTESIAN_POINT('',(0.,0.,0.));
#11189=CARTESIAN_POINT('',(0.,0.,0.));
#11190=CARTESIAN_POINT('',(0.,0.,0.));
#11191=CARTESIAN_POINT('',(0.,0.,0.));
#11192=CARTESIAN_POINT('',(0.,0.,0.));
#11193=CARTESIAN_POINT('',(0.,1.,8.));
#11194=CARTESIAN_POINT('',(-4.4,1.,2.5));
#11195=CARTESIAN_POINT('',(4.4,1.,2.5));
#11196=CARTESIAN_POINT('',(0.,5.,8.));
#11197=CARTESIAN_POINT('',(-4.4,5.,2.5));
#11198=CARTESIAN_POINT('',(4.4,5.,2.5));
#11199=CARTESIAN_POINT('',(3.3,-0.4,8.));
#11200=CARTESIAN_POINT('',(4.44089209850063E-16,-0.4,11.3));
#11201=CARTESIAN_POINT('',(-3.3,-0.4,8.));
#11202=CARTESIAN_POINT('',(-4.44089209850063E-16,-0.4,4.7));
#11203=CARTESIAN_POINT('',(3.3,6.4,8.));
#11204=CARTESIAN_POINT('',(4.44089209850063E-16,6.4,11.3));
#11205=CARTESIAN_POINT('',(-3.3,6.4,8.));
#11206=CARTESIAN_POINT('',(-4.44089209850063E-16,6.4,4.7));
#11207=CARTESIAN_POINT('',(0.,0.,0.));
#11208=CARTESIAN_POINT('',(0.,0.,0.));
#11209=CARTESIAN_POINT('Origin',(-0.4,7.8,6.6));
#11210=CARTESIAN_POINT('',(-0.4,9.8,6.8157280717673));
#11211=CARTESIAN_POINT('',(-0.4,7.8,6.8157280717673));
#11212=CARTESIAN_POINT('',(-0.4,-3.5,6.8157280717673));
#11213=CARTESIAN_POINT('',(-0.4,9.8,7.15));
#11214=CARTESIAN_POINT('',(-0.4,9.8,7.15));
#11215=CARTESIAN_POINT('',(-0.4,7.8,7.15));
#11216=CARTESIAN_POINT('',(-0.4,7.8,7.15));
#11217=CARTESIAN_POINT('',(-0.4,7.8,7.15));
#11218=CARTESIAN_POINT('Origin',(0.,7.8,6.875));
#11219=CARTESIAN_POINT('',(0.4,7.8,6.8157280717673));
#11220=CARTESIAN_POINT('Origin',(0.,7.8,8.));
#11221=CARTESIAN_POINT('',(0.4,7.8,7.15));
#11222=CARTESIAN_POINT('',(0.4,7.8,7.15));
#11223=CARTESIAN_POINT('',(0.4,7.8,6.6));
#11224=CARTESIAN_POINT('Origin',(0.4,7.8,7.15));
#11225=CARTESIAN_POINT('',(0.4,9.8,6.8157280717673));
#11226=CARTESIAN_POINT('',(0.4,-3.5,6.8157280717673));
#11227=CARTESIAN_POINT('',(0.4,9.8,7.15));
#11228=CARTESIAN_POINT('',(0.4,7.8,7.15));
#11229=CARTESIAN_POINT('',(0.4,9.8,6.6));
#11230=CARTESIAN_POINT('Origin',(-0.4,7.8,7.15));
#11231=CARTESIAN_POINT('',(0.4,9.8,7.15));
#11232=CARTESIAN_POINT('Origin',(0.,9.8,6.875));
#11233=CARTESIAN_POINT('Origin',(0.,9.8,8.));
#11234=CARTESIAN_POINT('Origin',(-0.4,-3.2,6.6));
#11235=CARTESIAN_POINT('',(-0.4,-1.2,6.8157280717673));
#11236=CARTESIAN_POINT('',(-0.4,-3.2,6.8157280717673));
#11237=CARTESIAN_POINT('',(-0.4,-3.5,6.8157280717673));
#11238=CARTESIAN_POINT('',(-0.4,-1.2,7.15));
#11239=CARTESIAN_POINT('',(-0.4,-1.2,7.15));
#11240=CARTESIAN_POINT('',(-0.4,-3.2,7.15));
#11241=CARTESIAN_POINT('',(-0.4,-3.2,7.15));
#11242=CARTESIAN_POINT('',(-0.4,-3.2,7.15));
#11243=CARTESIAN_POINT('Origin',(0.,-3.2,6.875));
#11244=CARTESIAN_POINT('',(0.4,-3.2,6.8157280717673));
#11245=CARTESIAN_POINT('Origin',(0.,-3.2,8.));
#11246=CARTESIAN_POINT('',(0.4,-3.2,7.15));
#11247=CARTESIAN_POINT('',(0.4,-3.2,7.15));
#11248=CARTESIAN_POINT('',(0.4,-3.2,6.6));
#11249=CARTESIAN_POINT('Origin',(0.4,-3.2,7.15));
#11250=CARTESIAN_POINT('',(0.4,-1.2,6.8157280717673));
#11251=CARTESIAN_POINT('',(0.4,-3.5,6.8157280717673));
#11252=CARTESIAN_POINT('',(0.4,-1.2,7.15));
#11253=CARTESIAN_POINT('',(0.4,-3.2,7.15));
#11254=CARTESIAN_POINT('',(0.4,-1.2,6.6));
#11255=CARTESIAN_POINT('Origin',(-0.4,-3.2,7.15));
#11256=CARTESIAN_POINT('',(0.4,-1.2,7.15));
#11257=CARTESIAN_POINT('Origin',(0.,-1.2,6.875));
#11258=CARTESIAN_POINT('Origin',(0.,-1.2,8.));
#11259=CARTESIAN_POINT('Origin',(0.,0.25,8.));
#11260=CARTESIAN_POINT('',(-1.6,0.25,8.));
#11261=CARTESIAN_POINT('Origin',(0.,0.25,8.));
#11262=CARTESIAN_POINT('',(-1.25,0.25,8.));
#11263=CARTESIAN_POINT('Origin',(0.,0.25,8.));
#11264=CARTESIAN_POINT('Origin',(0.,-0.1,8.));
#11265=CARTESIAN_POINT('',(-1.6,-0.1,8.));
#11266=CARTESIAN_POINT('Origin',(0.,-0.1,8.));
#11267=CARTESIAN_POINT('',(-1.25,-0.1,8.));
#11268=CARTESIAN_POINT('Origin',(0.,-0.1,8.));
#11269=CARTESIAN_POINT('Origin',(0.,-0.1,8.));
#11270=CARTESIAN_POINT('',(-1.6,-0.1,8.));
#11271=CARTESIAN_POINT('Origin',(0.,-3.5,8.));
#11272=CARTESIAN_POINT('',(-1.25,-3.5,8.));
#11273=CARTESIAN_POINT('',(-1.25,-3.5,8.));
#11274=CARTESIAN_POINT('Origin',(0.,-3.5,8.));
#11275=CARTESIAN_POINT('Origin',(0.,-3.5,8.));
#11276=CARTESIAN_POINT('',(-1.25,10.,8.));
#11277=CARTESIAN_POINT('Origin',(0.,10.,8.));
#11278=CARTESIAN_POINT('',(-1.25,-3.5,8.));
#11279=CARTESIAN_POINT('Origin',(0.,10.,8.));
#11280=CARTESIAN_POINT('Origin',(0.,-3.5,8.));
#11281=CARTESIAN_POINT('',(0.,0.,0.));
#11282=CARTESIAN_POINT('Origin',(0.,5.75,8.));
#11283=CARTESIAN_POINT('',(-1.255,6.4,8.));
#11284=CARTESIAN_POINT('Origin',(0.,6.4,8.));
#11285=CARTESIAN_POINT('',(-1.255,5.75,8.));
#11286=CARTESIAN_POINT('',(-1.255,5.75,8.));
#11287=CARTESIAN_POINT('Origin',(0.,5.75,8.));
#11288=CARTESIAN_POINT('Origin',(0.,5.75,8.));
#11289=CARTESIAN_POINT('',(-1.7,6.4,8.));
#11290=CARTESIAN_POINT('Origin',(0.,6.4,8.));
#11291=CARTESIAN_POINT('',(-1.7,5.75,8.));
#11292=CARTESIAN_POINT('',(-1.7,5.75,8.));
#11293=CARTESIAN_POINT('Origin',(0.,5.75,8.));
#11294=CARTESIAN_POINT('Origin',(0.,6.4,8.));
#11295=CARTESIAN_POINT('Origin',(0.,5.75,8.));
#11296=CARTESIAN_POINT('',(0.,0.,0.));
#11297=CARTESIAN_POINT('Origin',(0.,6.8,9.24));
#11298=CARTESIAN_POINT('',(0.193455421221531,6.71829932680816,9.24));
#11299=CARTESIAN_POINT('',(0.193455421221531,6.88170067319184,9.24));
#11300=CARTESIAN_POINT('',(0.193455421221531,6.4,9.24));
#11301=CARTESIAN_POINT('Origin',(0.,6.8,9.24));
#11302=CARTESIAN_POINT('Origin',(0.,6.8,9.24));
#11303=CARTESIAN_POINT('',(-0.193455421221531,6.71829932680816,9.24));
#11304=CARTESIAN_POINT('Ctrl Pts',(-0.193455421221531,6.71829932680816,
9.24));
#11305=CARTESIAN_POINT('Ctrl Pts',(-0.182741806873435,6.69293103184137,
9.24167145707784));
#11306=CARTESIAN_POINT('Ctrl Pts',(-0.166804849537961,6.66982000143961,
9.24400210952839));
#11307=CARTESIAN_POINT('Ctrl Pts',(-0.129875785635207,6.63289093753686,
9.24840249136865));
#11308=CARTESIAN_POINT('Ctrl Pts',(-0.106295060941802,6.6167372734261,9.2507589672592));
#11309=CARTESIAN_POINT('Ctrl Pts',(-0.0545698089447934,6.59529044194989,
9.25408084670822));
#11310=CARTESIAN_POINT('Ctrl Pts',(-0.0264211917910691,6.59,9.255));
#11311=CARTESIAN_POINT('Ctrl Pts',(0.026421191791069,6.59,9.255));
#11312=CARTESIAN_POINT('Ctrl Pts',(0.0545698089447934,6.59529044194989,
9.25408084670822));
#11313=CARTESIAN_POINT('Ctrl Pts',(0.106295060941802,6.6167372734261,9.2507589672592));
#11314=CARTESIAN_POINT('Ctrl Pts',(0.129875785635207,6.63289093753686,9.24840249136865));
#11315=CARTESIAN_POINT('Ctrl Pts',(0.166804849537961,6.66982000143961,9.24400210952839));
#11316=CARTESIAN_POINT('Ctrl Pts',(0.182741806873435,6.69293103184137,9.24167145707784));
#11317=CARTESIAN_POINT('Ctrl Pts',(0.193455421221531,6.71829932680816,9.24));
#11318=CARTESIAN_POINT('',(-0.21,6.8,9.24));
#11319=CARTESIAN_POINT('Origin',(0.,6.8,9.24));
#11320=CARTESIAN_POINT('',(-0.21,6.8,9.78770802985275));
#11321=CARTESIAN_POINT('',(-0.21,6.8,9.24));
#11322=CARTESIAN_POINT('',(0.21,6.8,9.78770802985275));
#11323=CARTESIAN_POINT('Ctrl Pts',(0.21,6.8,9.78770802985275));
#11324=CARTESIAN_POINT('Ctrl Pts',(0.21,6.77360603148425,9.78770802985275));
#11325=CARTESIAN_POINT('Ctrl Pts',(0.204720232951726,6.74546934556601,9.78835284034214));
#11326=CARTESIAN_POINT('Ctrl Pts',(0.183281523978899,6.69373688397397,9.79067700538683));
#11327=CARTESIAN_POINT('Ctrl Pts',(0.167123888882363,6.67013904078401,9.79232226897314));
#11328=CARTESIAN_POINT('Ctrl Pts',(0.129861077103665,6.63287622900531,9.79540680803063));
#11329=CARTESIAN_POINT('Ctrl Pts',(0.106263182528071,6.6167185016358,9.79704717240673));
#11330=CARTESIAN_POINT('Ctrl Pts',(0.0545305475112071,6.59527972468261,
9.79936011492601));
#11331=CARTESIAN_POINT('Ctrl Pts',(0.0263938015120406,6.59,9.8));
#11332=CARTESIAN_POINT('Ctrl Pts',(-0.0263938015120406,6.59,9.8));
#11333=CARTESIAN_POINT('Ctrl Pts',(-0.054530547511207,6.59527972468261,
9.79936011492601));
#11334=CARTESIAN_POINT('Ctrl Pts',(-0.106263182528071,6.6167185016358,9.79704717240673));
#11335=CARTESIAN_POINT('Ctrl Pts',(-0.129861077103665,6.63287622900531,
9.79540680803063));
#11336=CARTESIAN_POINT('Ctrl Pts',(-0.167123888882363,6.67013904078401,
9.79232226897314));
#11337=CARTESIAN_POINT('Ctrl Pts',(-0.183281523978899,6.69373688397397,
9.79067700538683));
#11338=CARTESIAN_POINT('Ctrl Pts',(-0.204720232951726,6.74546934556601,
9.78835284034214));
#11339=CARTESIAN_POINT('Ctrl Pts',(-0.21,6.77360603148425,9.78770802985275));
#11340=CARTESIAN_POINT('Ctrl Pts',(-0.21,6.8,9.78770802985275));
#11341=CARTESIAN_POINT('Ctrl Pts',(-0.21,6.8,9.78770802985275));
#11342=CARTESIAN_POINT('Ctrl Pts',(-0.21,6.82639396851575,9.78770802985275));
#11343=CARTESIAN_POINT('Ctrl Pts',(-0.204720232951726,6.85453065443398,
9.78835284034214));
#11344=CARTESIAN_POINT('Ctrl Pts',(-0.1832815239789,6.90626311602603,9.79067700538683));
#11345=CARTESIAN_POINT('Ctrl Pts',(-0.167123888882363,6.92986095921599,
9.79232226897314));
#11346=CARTESIAN_POINT('Ctrl Pts',(-0.129861077103665,6.96712377099468,
9.79540680803063));
#11347=CARTESIAN_POINT('Ctrl Pts',(-0.106263182528071,6.9832814983642,9.79704717240673));
#11348=CARTESIAN_POINT('Ctrl Pts',(-0.0545305475112072,7.00472027531739,
9.79936011492601));
#11349=CARTESIAN_POINT('Ctrl Pts',(-0.0263938015120407,7.01,9.8));
#11350=CARTESIAN_POINT('Ctrl Pts',(0.0263938015120407,7.01,9.8));
#11351=CARTESIAN_POINT('Ctrl Pts',(0.0545305475112071,7.00472027531739,
9.79936011492601));
#11352=CARTESIAN_POINT('Ctrl Pts',(0.106263182528071,6.9832814983642,9.79704717240673));
#11353=CARTESIAN_POINT('Ctrl Pts',(0.129861077103665,6.96712377099468,9.79540680803063));
#11354=CARTESIAN_POINT('Ctrl Pts',(0.167123888882363,6.92986095921599,9.79232226897314));
#11355=CARTESIAN_POINT('Ctrl Pts',(0.1832815239789,6.90626311602603,9.79067700538683));
#11356=CARTESIAN_POINT('Ctrl Pts',(0.204720232951726,6.85453065443398,9.78835284034214));
#11357=CARTESIAN_POINT('Ctrl Pts',(0.21,6.82639396851575,9.78770802985275));
#11358=CARTESIAN_POINT('Ctrl Pts',(0.21,6.8,9.78770802985275));
#11359=CARTESIAN_POINT('',(-0.193455421221531,6.88170067319184,9.24));
#11360=CARTESIAN_POINT('Origin',(0.,6.8,9.24));
#11361=CARTESIAN_POINT('Ctrl Pts',(0.19345542122153,6.88170067319184,9.24));
#11362=CARTESIAN_POINT('Ctrl Pts',(0.182741806873435,6.90706896815863,9.24167145707784));
#11363=CARTESIAN_POINT('Ctrl Pts',(0.166804849537961,6.93017999856039,9.24400210952839));
#11364=CARTESIAN_POINT('Ctrl Pts',(0.129875785635207,6.96710906246314,9.24840249136865));
#11365=CARTESIAN_POINT('Ctrl Pts',(0.106295060941802,6.9832627265739,9.2507589672592));
#11366=CARTESIAN_POINT('Ctrl Pts',(0.0545698089447934,7.0047095580501,9.25408084670822));
#11367=CARTESIAN_POINT('Ctrl Pts',(0.026421191791069,7.01,9.255));
#11368=CARTESIAN_POINT('Ctrl Pts',(-0.026421191791069,7.01,9.255));
#11369=CARTESIAN_POINT('Ctrl Pts',(-0.0545698089447934,7.0047095580501,
9.25408084670822));
#11370=CARTESIAN_POINT('Ctrl Pts',(-0.106295060941802,6.9832627265739,9.2507589672592));
#11371=CARTESIAN_POINT('Ctrl Pts',(-0.129875785635207,6.96710906246314,
9.24840249136865));
#11372=CARTESIAN_POINT('Ctrl Pts',(-0.166804849537961,6.93017999856039,
9.24400210952839));
#11373=CARTESIAN_POINT('Ctrl Pts',(-0.182741806873435,6.90706896815863,
9.24167145707784));
#11374=CARTESIAN_POINT('Ctrl Pts',(-0.19345542122153,6.88170067319184,9.24));
#11375=CARTESIAN_POINT('Origin',(0.,6.8,9.24));
#11376=CARTESIAN_POINT('',(-0.193455421221531,6.4,9.24));
#11377=CARTESIAN_POINT('Origin',(0.,6.4,8.));
#11378=CARTESIAN_POINT('',(-1.255,7.2,8.));
#11379=CARTESIAN_POINT('Origin',(0.,7.2,8.));
#11380=CARTESIAN_POINT('',(-1.255,6.4,8.));
#11381=CARTESIAN_POINT('',(-1.255,6.4,8.));
#11382=CARTESIAN_POINT('Origin',(0.,6.4,8.));
#11383=CARTESIAN_POINT('Origin',(0.,6.4,8.));
#11384=CARTESIAN_POINT('',(-1.8,7.2,8.));
#11385=CARTESIAN_POINT('Origin',(0.,7.2,8.));
#11386=CARTESIAN_POINT('',(-1.8,6.4,8.));
#11387=CARTESIAN_POINT('',(-1.8,6.4,8.));
#11388=CARTESIAN_POINT('Origin',(0.,6.4,8.));
#11389=CARTESIAN_POINT('Origin',(0.,7.2,8.));
#11390=CARTESIAN_POINT('Origin',(0.,6.4,8.));
#11391=CARTESIAN_POINT('',(0.,0.,0.));
#11392=CARTESIAN_POINT('Origin',(0.,-2.2,9.24));
#11393=CARTESIAN_POINT('',(0.157797338380593,-2.33856406460551,9.24));
#11394=CARTESIAN_POINT('',(0.157797338380593,-2.06143593539449,9.24));
#11395=CARTESIAN_POINT('',(0.157797338380593,-4.,9.24));
#11396=CARTESIAN_POINT('Origin',(0.,-2.2,9.24));
#11397=CARTESIAN_POINT('Origin',(0.,-2.2,9.24));
#11398=CARTESIAN_POINT('',(-0.157797338380593,-2.33856406460551,9.24));
#11399=CARTESIAN_POINT('Ctrl Pts',(-0.157797338380593,-2.33856406460551,
9.24));
#11400=CARTESIAN_POINT('Ctrl Pts',(-0.154774443077063,-2.34200655046545,
9.24038468131702));
#11401=CARTESIAN_POINT('Ctrl Pts',(-0.151666037725851,-2.3453188103725,
9.24076896680743));
#11402=CARTESIAN_POINT('Ctrl Pts',(-0.129876016991637,-2.36710883110671,
9.24337594943507));
#11403=CARTESIAN_POINT('Ctrl Pts',(-0.1062955610194,-2.38326243211879,9.24574191032087));
#11404=CARTESIAN_POINT('Ctrl Pts',(-0.0545704238568476,-2.4047093901954,
9.24907714823024));
#11405=CARTESIAN_POINT('Ctrl Pts',(-0.0264216205957885,-2.41,9.25));
#11406=CARTESIAN_POINT('Ctrl Pts',(0.0264216205957884,-2.41,9.25));
#11407=CARTESIAN_POINT('Ctrl Pts',(0.0545704238568477,-2.4047093901954,
9.24907714823024));
#11408=CARTESIAN_POINT('Ctrl Pts',(0.106295561019401,-2.38326243211879,
9.24574191032086));
#11409=CARTESIAN_POINT('Ctrl Pts',(0.129876016991637,-2.36710883110671,
9.24337594943507));
#11410=CARTESIAN_POINT('Ctrl Pts',(0.151666037725851,-2.3453188103725,9.24076896680743));
#11411=CARTESIAN_POINT('Ctrl Pts',(0.154774443077063,-2.34200655046545,
9.24038468131702));
#11412=CARTESIAN_POINT('Ctrl Pts',(0.157797338380593,-2.33856406460551,
9.24));
#11413=CARTESIAN_POINT('',(-0.21,-2.2,9.24));
#11414=CARTESIAN_POINT('Origin',(0.,-2.2,9.24));
#11415=CARTESIAN_POINT('',(-0.21,-2.2,9.98894444366855));
#11416=CARTESIAN_POINT('',(-0.21,-2.2,9.24));
#11417=CARTESIAN_POINT('',(0.21,-2.2,9.98894444366855));
#11418=CARTESIAN_POINT('Ctrl Pts',(0.21,-2.2,9.98894444366855));
#11419=CARTESIAN_POINT('Ctrl Pts',(0.21,-2.22638900835931,9.98894444366855));
#11420=CARTESIAN_POINT('Ctrl Pts',(0.204722164681422,-2.25452359377817,
9.98952376620524));
#11421=CARTESIAN_POINT('Ctrl Pts',(0.183284867450471,-2.30625744682115,
9.99161307432363));
#11422=CARTESIAN_POINT('Ctrl Pts',(0.167126466290584,-2.32985838180777,
9.99309254589373));
#11423=CARTESIAN_POINT('Ctrl Pts',(0.129858458976497,-2.36712638912185,
9.99586721250997));
#11424=CARTESIAN_POINT('Ctrl Pts',(0.106257490219278,-2.38328485056549,
9.997343117591));
#11425=CARTESIAN_POINT('Ctrl Pts',(0.0545235237847868,-2.40472219258686,
9.99942425936951));
#11426=CARTESIAN_POINT('Ctrl Pts',(0.0263888990751172,-2.41,10.));
#11427=CARTESIAN_POINT('Ctrl Pts',(-0.0263888990751171,-2.41,10.));
#11428=CARTESIAN_POINT('Ctrl Pts',(-0.0545235237847868,-2.40472219258686,
9.99942425936951));
#11429=CARTESIAN_POINT('Ctrl Pts',(-0.106257490219278,-2.38328485056549,
9.997343117591));
#11430=CARTESIAN_POINT('Ctrl Pts',(-0.129858458976497,-2.36712638912185,
9.99586721250997));
#11431=CARTESIAN_POINT('Ctrl Pts',(-0.167126466290584,-2.32985838180777,
9.99309254589373));
#11432=CARTESIAN_POINT('Ctrl Pts',(-0.183284867450471,-2.30625744682115,
9.99161307432363));
#11433=CARTESIAN_POINT('Ctrl Pts',(-0.204722164681422,-2.25452359377817,
9.98952376620524));
#11434=CARTESIAN_POINT('Ctrl Pts',(-0.21,-2.22638900835931,9.98894444366855));
#11435=CARTESIAN_POINT('Ctrl Pts',(-0.21,-2.2,9.98894444366855));
#11436=CARTESIAN_POINT('Ctrl Pts',(-0.21,-2.2,9.98894444366855));
#11437=CARTESIAN_POINT('Ctrl Pts',(-0.21,-2.17361099164069,9.98894444366855));
#11438=CARTESIAN_POINT('Ctrl Pts',(-0.204722164681422,-2.14547640622183,
9.98952376620524));
#11439=CARTESIAN_POINT('Ctrl Pts',(-0.183284867450471,-2.09374255317885,
9.99161307432363));
#11440=CARTESIAN_POINT('Ctrl Pts',(-0.167126466290584,-2.07014161819223,
9.99309254589373));
#11441=CARTESIAN_POINT('Ctrl Pts',(-0.129858458976497,-2.03287361087815,
9.99586721250997));
#11442=CARTESIAN_POINT('Ctrl Pts',(-0.106257490219278,-2.01671514943451,
9.997343117591));
#11443=CARTESIAN_POINT('Ctrl Pts',(-0.0545235237847867,-1.99527780741314,
9.99942425936951));
#11444=CARTESIAN_POINT('Ctrl Pts',(-0.0263888990751172,-1.99,10.));
#11445=CARTESIAN_POINT('Ctrl Pts',(0.0263888990751171,-1.99,10.));
#11446=CARTESIAN_POINT('Ctrl Pts',(0.0545235237847866,-1.99527780741314,
9.99942425936951));
#11447=CARTESIAN_POINT('Ctrl Pts',(0.106257490219277,-2.01671514943451,
9.997343117591));
#11448=CARTESIAN_POINT('Ctrl Pts',(0.129858458976496,-2.03287361087815,
9.99586721250997));
#11449=CARTESIAN_POINT('Ctrl Pts',(0.167126466290584,-2.07014161819223,
9.99309254589373));
#11450=CARTESIAN_POINT('Ctrl Pts',(0.183284867450471,-2.09374255317885,
9.99161307432363));
#11451=CARTESIAN_POINT('Ctrl Pts',(0.204722164681422,-2.14547640622183,
9.98952376620524));
#11452=CARTESIAN_POINT('Ctrl Pts',(0.21,-2.17361099164069,9.98894444366855));
#11453=CARTESIAN_POINT('Ctrl Pts',(0.21,-2.2,9.98894444366855));
#11454=CARTESIAN_POINT('',(-0.157797338380593,-2.06143593539449,9.24));
#11455=CARTESIAN_POINT('Origin',(0.,-2.2,9.24));
#11456=CARTESIAN_POINT('Ctrl Pts',(0.157797338380593,-2.06143593539449,
9.24));
#11457=CARTESIAN_POINT('Ctrl Pts',(0.154774443077063,-2.05799344953455,
9.24038468131702));
#11458=CARTESIAN_POINT('Ctrl Pts',(0.151666037725851,-2.0546811896275,9.24076896680743));
#11459=CARTESIAN_POINT('Ctrl Pts',(0.129876016991637,-2.03289116889329,
9.24337594943507));
#11460=CARTESIAN_POINT('Ctrl Pts',(0.1062955610194,-2.01673756788121,9.24574191032087));
#11461=CARTESIAN_POINT('Ctrl Pts',(0.0545704238568475,-1.9952906098046,
9.24907714823024));
#11462=CARTESIAN_POINT('Ctrl Pts',(0.0264216205957885,-1.99,9.25));
#11463=CARTESIAN_POINT('Ctrl Pts',(-0.0264216205957884,-1.99,9.25));
#11464=CARTESIAN_POINT('Ctrl Pts',(-0.0545704238568475,-1.9952906098046,
9.24907714823024));
#11465=CARTESIAN_POINT('Ctrl Pts',(-0.1062955610194,-2.01673756788121,9.24574191032087));
#11466=CARTESIAN_POINT('Ctrl Pts',(-0.129876016991637,-2.03289116889329,
9.24337594943507));
#11467=CARTESIAN_POINT('Ctrl Pts',(-0.151666037725851,-2.0546811896275,
9.24076896680743));
#11468=CARTESIAN_POINT('Ctrl Pts',(-0.154774443077063,-2.05799344953455,
9.24038468131702));
#11469=CARTESIAN_POINT('Ctrl Pts',(-0.157797338380593,-2.06143593539449,
9.24));
#11470=CARTESIAN_POINT('Origin',(0.,-2.2,9.24));
#11471=CARTESIAN_POINT('',(-0.157797338380593,-4.,9.24));
#11472=CARTESIAN_POINT('Origin',(0.4,-4.1,6.42));
#11473=CARTESIAN_POINT('',(-0.4,-0.5,6.42));
#11474=CARTESIAN_POINT('',(0.4,-0.5,6.42));
#11475=CARTESIAN_POINT('',(0.2,-0.5,6.42));
#11476=CARTESIAN_POINT('',(-0.4,-4.1,6.42));
#11477=CARTESIAN_POINT('',(-0.4,-4.1,6.42));
#11478=CARTESIAN_POINT('',(0.4,-4.1,6.42));
#11479=CARTESIAN_POINT('',(-0.4,-4.1,6.42));
#11480=CARTESIAN_POINT('',(0.4,-4.1,6.42));
#11481=CARTESIAN_POINT('Origin',(0.4,-4.1,8.));
#11482=CARTESIAN_POINT('',(0.4,-0.5,6.8157280717673));
#11483=CARTESIAN_POINT('',(0.4,-0.5,8.));
#11484=CARTESIAN_POINT('',(0.4,-4.1,8.));
#11485=CARTESIAN_POINT('',(0.4,-4.1,6.42));
#11486=CARTESIAN_POINT('',(0.4,-4.,8.));
#11487=CARTESIAN_POINT('',(0.4,-4.1,8.));
#11488=CARTESIAN_POINT('',(0.4,-4.,6.8157280717673));
#11489=CARTESIAN_POINT('',(0.4,-4.,8.));
#11490=CARTESIAN_POINT('',(0.4,-4.,6.8157280717673));
#11491=CARTESIAN_POINT('Origin',(-0.4,-4.1,6.42));
#11492=CARTESIAN_POINT('',(-0.4,-0.5,6.8157280717673));
#11493=CARTESIAN_POINT('',(-0.4,-0.5,7.21));
#11494=CARTESIAN_POINT('',(-0.4,-4.,6.8157280717673));
#11495=CARTESIAN_POINT('',(-0.4,-4.,6.8157280717673));
#11496=CARTESIAN_POINT('',(-0.4,-4.,8.));
#11497=CARTESIAN_POINT('',(-0.4,-4.,7.21));
#11498=CARTESIAN_POINT('',(-0.4,-4.1,8.));
#11499=CARTESIAN_POINT('',(-0.4,-4.1,8.));
#11500=CARTESIAN_POINT('',(-0.4,-4.1,8.));
#11501=CARTESIAN_POINT('Origin',(-0.4,-4.1,8.));
#11502=CARTESIAN_POINT('',(-0.2,-4.,8.));
#11503=CARTESIAN_POINT('',(0.4,-4.1,8.));
#11504=CARTESIAN_POINT('Origin',(0.,-4.1,7.21));
#11505=CARTESIAN_POINT('Origin',(0.,-0.5,8.));
#11506=CARTESIAN_POINT('',(-2.,-0.5,8.));
#11507=CARTESIAN_POINT('Origin',(0.,-0.5,8.));
#11508=CARTESIAN_POINT('Origin',(0.,-0.5,8.));
#11509=CARTESIAN_POINT('Origin',(-0.635,-6.,7.365));
#11510=CARTESIAN_POINT('',(-0.635,-6.,8.635));
#11511=CARTESIAN_POINT('',(-0.635,-6.,7.365));
#11512=CARTESIAN_POINT('',(-0.635,-6.,8.635));
#11513=CARTESIAN_POINT('',(-0.635,-4.3,8.635));
#11514=CARTESIAN_POINT('',(-0.635,-6.,8.635));
#11515=CARTESIAN_POINT('',(-0.635,-4.3,7.365));
#11516=CARTESIAN_POINT('',(-0.635,-4.3,7.6825));
#11517=CARTESIAN_POINT('',(-0.635,-6.,7.365));
#11518=CARTESIAN_POINT('Origin',(0.635,-6.,7.365));
#11519=CARTESIAN_POINT('',(0.635,-6.,7.365));
#11520=CARTESIAN_POINT('',(-0.635,-6.,7.365));
#11521=CARTESIAN_POINT('',(0.635,-4.3,7.365));
#11522=CARTESIAN_POINT('',(0.3175,-4.3,7.365));
#11523=CARTESIAN_POINT('',(0.635,-6.,7.365));
#11524=CARTESIAN_POINT('Origin',(0.635,-6.,8.635));
#11525=CARTESIAN_POINT('',(0.635,-6.,8.635));
#11526=CARTESIAN_POINT('',(0.635,-6.,7.365));
#11527=CARTESIAN_POINT('',(0.635,-4.3,8.635));
#11528=CARTESIAN_POINT('',(0.635,-4.3,8.3175));
#11529=CARTESIAN_POINT('',(0.635,-6.,8.635));
#11530=CARTESIAN_POINT('Origin',(-0.635,-6.,8.635));
#11531=CARTESIAN_POINT('',(0.635,-6.,8.635));
#11532=CARTESIAN_POINT('',(-0.3175,-4.3,8.635));
#11533=CARTESIAN_POINT('Origin',(0.,-6.,8.));
#11534=CARTESIAN_POINT('Origin',(0.,-4.,8.));
#11535=CARTESIAN_POINT('Origin',(0.,-4.,8.));
#11536=CARTESIAN_POINT('Origin',(0.,-4.3,8.));
#11537=CARTESIAN_POINT('',(-2.,-4.3,8.));
#11538=CARTESIAN_POINT('Origin',(0.,-4.3,8.));
#11539=CARTESIAN_POINT('Origin',(0.,-4.,8.));
#11540=CARTESIAN_POINT('Origin',(0.,-4.,8.));
#11541=CARTESIAN_POINT('',(-2.,-4.,8.));
#11542=CARTESIAN_POINT('',(0.,0.,0.));
#11543=CARTESIAN_POINT('Origin',(0.,8.8,9.24));
#11544=CARTESIAN_POINT('',(0.157797338380593,8.66143593539449,9.24));
#11545=CARTESIAN_POINT('',(0.157797338380593,8.93856406460551,9.24));
#11546=CARTESIAN_POINT('',(0.157797338380593,7.4,9.24));
#11547=CARTESIAN_POINT('Origin',(0.,8.8,9.24));
#11548=CARTESIAN_POINT('Origin',(0.,8.8,9.24));
#11549=CARTESIAN_POINT('',(-0.157797338380593,8.66143593539449,9.24));
#11550=CARTESIAN_POINT('Ctrl Pts',(-0.157797338380593,8.66143593539449,
9.24));
#11551=CARTESIAN_POINT('Ctrl Pts',(-0.154774443077063,8.65799344953455,
9.24038468131702));
#11552=CARTESIAN_POINT('Ctrl Pts',(-0.151666037725851,8.6546811896275,9.24076896680743));
#11553=CARTESIAN_POINT('Ctrl Pts',(-0.129876016991636,8.63289116889329,
9.24337594943507));
#11554=CARTESIAN_POINT('Ctrl Pts',(-0.1062955610194,8.61673756788121,9.24574191032087));
#11555=CARTESIAN_POINT('Ctrl Pts',(-0.054570423856847,8.59529060980459,
9.24907714823024));
#11556=CARTESIAN_POINT('Ctrl Pts',(-0.0264216205957885,8.59,9.25));
#11557=CARTESIAN_POINT('Ctrl Pts',(0.0264216205957884,8.59,9.25));
#11558=CARTESIAN_POINT('Ctrl Pts',(0.054570423856847,8.59529060980459,9.24907714823024));
#11559=CARTESIAN_POINT('Ctrl Pts',(0.1062955610194,8.61673756788121,9.24574191032087));
#11560=CARTESIAN_POINT('Ctrl Pts',(0.129876016991636,8.63289116889329,9.24337594943507));
#11561=CARTESIAN_POINT('Ctrl Pts',(0.151666037725851,8.6546811896275,9.24076896680743));
#11562=CARTESIAN_POINT('Ctrl Pts',(0.154774443077063,8.65799344953455,9.24038468131702));
#11563=CARTESIAN_POINT('Ctrl Pts',(0.157797338380593,8.66143593539449,9.24));
#11564=CARTESIAN_POINT('',(-0.21,8.8,9.24));
#11565=CARTESIAN_POINT('Origin',(0.,8.8,9.24));
#11566=CARTESIAN_POINT('',(-0.21,8.8,10.4911643863864));
#11567=CARTESIAN_POINT('',(-0.21,8.8,9.24));
#11568=CARTESIAN_POINT('',(0.21,8.8,10.4911643863864));
#11569=CARTESIAN_POINT('Ctrl Pts',(0.21,8.8,10.4911643863864));
#11570=CARTESIAN_POINT('Ctrl Pts',(0.21,8.77361856819303,10.4911643863864));
#11571=CARTESIAN_POINT('Ctrl Pts',(0.204725118204866,8.74548720786942,10.4916266149403));
#11572=CARTESIAN_POINT('Ctrl Pts',(0.183289989572642,8.69375124157695,10.4932950771364));
#11573=CARTESIAN_POINT('Ctrl Pts',(0.16713042375487,8.67014557565652,10.4944771047991));
#11574=CARTESIAN_POINT('Ctrl Pts',(0.129854455840894,8.63286960774255,10.4966951003339));
#11575=CARTESIAN_POINT('Ctrl Pts',(0.106248776012194,8.61671001748363,10.4978753058977));
#11576=CARTESIAN_POINT('Ctrl Pts',(0.0545127635959799,8.59527487020396,
10.4995395985687));
#11577=CARTESIAN_POINT('Ctrl Pts',(0.0263813872234849,8.59,10.5));
#11578=CARTESIAN_POINT('Ctrl Pts',(-0.0263813872234849,8.59,10.5));
#11579=CARTESIAN_POINT('Ctrl Pts',(-0.0545127635959799,8.59527487020396,
10.4995395985687));
#11580=CARTESIAN_POINT('Ctrl Pts',(-0.106248776012194,8.61671001748363,
10.4978753058977));
#11581=CARTESIAN_POINT('Ctrl Pts',(-0.129854455840894,8.63286960774255,
10.4966951003339));
#11582=CARTESIAN_POINT('Ctrl Pts',(-0.16713042375487,8.67014557565652,10.4944771047991));
#11583=CARTESIAN_POINT('Ctrl Pts',(-0.183289989572642,8.69375124157695,
10.4932950771364));
#11584=CARTESIAN_POINT('Ctrl Pts',(-0.204725118204866,8.74548720786942,
10.4916266149403));
#11585=CARTESIAN_POINT('Ctrl Pts',(-0.21,8.77361856819304,10.4911643863864));
#11586=CARTESIAN_POINT('Ctrl Pts',(-0.21,8.8,10.4911643863864));
#11587=CARTESIAN_POINT('Ctrl Pts',(-0.21,8.8,10.4911643863864));
#11588=CARTESIAN_POINT('Ctrl Pts',(-0.21,8.82638143180696,10.4911643863864));
#11589=CARTESIAN_POINT('Ctrl Pts',(-0.204725118204866,8.85451279213058,
10.4916266149403));
#11590=CARTESIAN_POINT('Ctrl Pts',(-0.183289989572642,8.90624875842305,
10.4932950771364));
#11591=CARTESIAN_POINT('Ctrl Pts',(-0.16713042375487,8.92985442434348,10.4944771047991));
#11592=CARTESIAN_POINT('Ctrl Pts',(-0.129854455840894,8.96713039225746,
10.4966951003339));
#11593=CARTESIAN_POINT('Ctrl Pts',(-0.106248776012194,8.98328998251637,
10.4978753058977));
#11594=CARTESIAN_POINT('Ctrl Pts',(-0.05451276359598,9.00472512979604,10.4995395985687));
#11595=CARTESIAN_POINT('Ctrl Pts',(-0.026381387223485,9.01,10.5));
#11596=CARTESIAN_POINT('Ctrl Pts',(0.0263813872234849,9.01,10.5));
#11597=CARTESIAN_POINT('Ctrl Pts',(0.0545127635959799,9.00472512979604,
10.4995395985687));
#11598=CARTESIAN_POINT('Ctrl Pts',(0.106248776012194,8.98328998251637,10.4978753058977));
#11599=CARTESIAN_POINT('Ctrl Pts',(0.129854455840894,8.96713039225746,10.4966951003339));
#11600=CARTESIAN_POINT('Ctrl Pts',(0.16713042375487,8.92985442434348,10.4944771047991));
#11601=CARTESIAN_POINT('Ctrl Pts',(0.183289989572642,8.90624875842305,10.4932950771364));
#11602=CARTESIAN_POINT('Ctrl Pts',(0.204725118204866,8.85451279213058,10.4916266149403));
#11603=CARTESIAN_POINT('Ctrl Pts',(0.21,8.82638143180697,10.4911643863864));
#11604=CARTESIAN_POINT('Ctrl Pts',(0.21,8.8,10.4911643863864));
#11605=CARTESIAN_POINT('',(-0.157797338380593,8.93856406460551,9.24));
#11606=CARTESIAN_POINT('Origin',(0.,8.8,9.24));
#11607=CARTESIAN_POINT('Ctrl Pts',(0.157797338380593,8.93856406460551,9.24));
#11608=CARTESIAN_POINT('Ctrl Pts',(0.154774443077063,8.94200655046545,9.24038468131702));
#11609=CARTESIAN_POINT('Ctrl Pts',(0.151666037725851,8.9453188103725,9.24076896680743));
#11610=CARTESIAN_POINT('Ctrl Pts',(0.129876016991636,8.96710883110671,9.24337594943507));
#11611=CARTESIAN_POINT('Ctrl Pts',(0.1062955610194,8.98326243211879,9.24574191032087));
#11612=CARTESIAN_POINT('Ctrl Pts',(0.054570423856847,9.00470939019541,9.24907714823024));
#11613=CARTESIAN_POINT('Ctrl Pts',(0.0264216205957885,9.01,9.25));
#11614=CARTESIAN_POINT('Ctrl Pts',(-0.0264216205957884,9.01,9.25));
#11615=CARTESIAN_POINT('Ctrl Pts',(-0.054570423856847,9.00470939019541,
9.24907714823024));
#11616=CARTESIAN_POINT('Ctrl Pts',(-0.1062955610194,8.98326243211879,9.24574191032087));
#11617=CARTESIAN_POINT('Ctrl Pts',(-0.129876016991636,8.96710883110671,
9.24337594943507));
#11618=CARTESIAN_POINT('Ctrl Pts',(-0.151666037725851,8.9453188103725,9.24076896680743));
#11619=CARTESIAN_POINT('Ctrl Pts',(-0.154774443077063,8.94200655046545,
9.24038468131702));
#11620=CARTESIAN_POINT('Ctrl Pts',(-0.157797338380593,8.93856406460551,
9.24));
#11621=CARTESIAN_POINT('Origin',(0.,8.8,9.24));
#11622=CARTESIAN_POINT('',(-0.157797338380593,7.4,9.24));
#11623=CARTESIAN_POINT('Origin',(-0.4,7.3,6.42));
#11624=CARTESIAN_POINT('',(-0.4,7.4,6.42));
#11625=CARTESIAN_POINT('',(-0.4,7.4,6.8157280717673));
#11626=CARTESIAN_POINT('',(-0.4,7.4,7.21));
#11627=CARTESIAN_POINT('',(-0.4,10.,6.42));
#11628=CARTESIAN_POINT('',(-0.4,7.3,6.42));
#11629=CARTESIAN_POINT('',(-0.4,10.,6.8157280717673));
#11630=CARTESIAN_POINT('',(-0.4,10.,7.21));
#11631=CARTESIAN_POINT('',(-0.4,7.4,6.8157280717673));
#11632=CARTESIAN_POINT('Origin',(0.4,7.3,6.42));
#11633=CARTESIAN_POINT('',(0.4,7.4,6.42));
#11634=CARTESIAN_POINT('',(0.2,7.4,6.42));
#11635=CARTESIAN_POINT('',(0.4,10.,6.42));
#11636=CARTESIAN_POINT('',(0.4,7.3,6.42));
#11637=CARTESIAN_POINT('',(0.2,10.,6.42));
#11638=CARTESIAN_POINT('Origin',(0.4,7.3,8.));
#11639=CARTESIAN_POINT('',(0.4,7.4,6.8157280717673));
#11640=CARTESIAN_POINT('',(0.4,7.4,8.));
#11641=CARTESIAN_POINT('',(0.4,10.,6.8157280717673));
#11642=CARTESIAN_POINT('',(0.4,7.4,6.8157280717673));
#11643=CARTESIAN_POINT('',(0.4,10.,8.));
#11644=CARTESIAN_POINT('Origin',(0.,10.,8.));
#11645=CARTESIAN_POINT('',(-2.5,10.,8.));
#11646=CARTESIAN_POINT('Origin',(0.,10.,8.));
#11647=CARTESIAN_POINT('Origin',(0.,10.,8.));
#11648=CARTESIAN_POINT('Origin',(0.,7.4,8.));
#11649=CARTESIAN_POINT('Origin',(0.,7.4,8.));
#11650=CARTESIAN_POINT('Origin',(50.,7.9,8.));
#11651=CARTESIAN_POINT('',(48.5,8.,8.));
#11652=CARTESIAN_POINT('Origin',(50.,8.,8.));
#11653=CARTESIAN_POINT('',(48.5,9.,8.));
#11654=CARTESIAN_POINT('',(48.5,7.9,8.));
#11655=CARTESIAN_POINT('Origin',(50.,9.,8.));
#11656=CARTESIAN_POINT('Origin',(50.,8.,8.));
#11657=CARTESIAN_POINT('',(48.2679491924311,9.,7.));
#11658=CARTESIAN_POINT('',(48.2679491924311,8.,7.));
#11659=CARTESIAN_POINT('',(48.2679491924311,8.,7.));
#11660=CARTESIAN_POINT('',(48.2679491924311,9.,9.));
#11661=CARTESIAN_POINT('Origin',(50.,9.,8.));
#11662=CARTESIAN_POINT('',(48.2679491924311,8.,9.));
#11663=CARTESIAN_POINT('',(48.2679491924311,8.,9.));
#11664=CARTESIAN_POINT('Origin',(50.,8.,8.));
#11665=CARTESIAN_POINT('Origin',(25.75,8.,8.));
#11666=CARTESIAN_POINT('',(2.29128784747792,8.,9.));
#11667=CARTESIAN_POINT('',(50.,8.,9.));
#11668=CARTESIAN_POINT('',(2.29128784747792,8.,7.));
#11669=CARTESIAN_POINT('Origin',(0.,8.,8.));
#11670=CARTESIAN_POINT('',(1.5,8.,7.));
#11671=CARTESIAN_POINT('Origin',(1.5,8.,9.));
#11672=CARTESIAN_POINT('',(2.29128784747792,9.,9.));
#11673=CARTESIAN_POINT('',(50.,9.,9.));
#11674=CARTESIAN_POINT('',(2.29128784747792,7.4,9.));
#11675=CARTESIAN_POINT('Origin',(25.75,9.,8.));
#11676=CARTESIAN_POINT('',(2.29128784747792,9.,7.));
#11677=CARTESIAN_POINT('',(1.5,9.,7.));
#11678=CARTESIAN_POINT('Origin',(0.,9.,8.));
#11679=CARTESIAN_POINT('Origin',(50.,8.,7.));
#11680=CARTESIAN_POINT('',(2.29128784747792,7.4,7.));
#11681=CARTESIAN_POINT('Origin',(0.,7.4,8.));
#11682=CARTESIAN_POINT('',(-2.5,7.4,8.));
#11683=CARTESIAN_POINT('',(-2.5,7.4,8.));
#11684=CARTESIAN_POINT('Origin',(0.,7.4,8.));
#11685=CARTESIAN_POINT('Origin',(0.,7.4,8.));
#11686=CARTESIAN_POINT('',(0.,0.,0.));
#11687=CARTESIAN_POINT('Origin',(50.,8.,8.));
#11688=CARTESIAN_POINT('',(48.5,8.05,8.));
#11689=CARTESIAN_POINT('Origin',(50.,8.05,8.));
#11690=CARTESIAN_POINT('',(48.5,8.,8.));
#11691=CARTESIAN_POINT('',(48.5,8.,8.));
#11692=CARTESIAN_POINT('Origin',(50.,8.,8.));
#11693=CARTESIAN_POINT('Origin',(50.,8.05,8.));
#11694=CARTESIAN_POINT('',(48.9,8.05,8.));
#11695=CARTESIAN_POINT('Origin',(50.,8.05,8.));
#11696=CARTESIAN_POINT('Origin',(50.,7.8,8.));
#11697=CARTESIAN_POINT('',(48.9,7.8,8.));
#11698=CARTESIAN_POINT('',(48.9,7.8,8.));
#11699=CARTESIAN_POINT('Origin',(50.,7.8,8.));
#11700=CARTESIAN_POINT('Origin',(50.,7.8,8.));
#11701=CARTESIAN_POINT('',(48.,8.,8.));
#11702=CARTESIAN_POINT('Origin',(50.,8.,8.));
#11703=CARTESIAN_POINT('',(48.,7.8,8.));
#11704=CARTESIAN_POINT('',(48.,7.8,8.));
#11705=CARTESIAN_POINT('Origin',(50.,7.8,8.));
#11706=CARTESIAN_POINT('Origin',(50.,8.,8.));
#11707=CARTESIAN_POINT('Origin',(50.,7.8,8.));
#11708=CARTESIAN_POINT('',(0.,0.,0.));
#11709=CARTESIAN_POINT('Origin',(50.,8.95,8.));
#11710=CARTESIAN_POINT('',(48.5,9.,8.));
#11711=CARTESIAN_POINT('Origin',(50.,9.,8.));
#11712=CARTESIAN_POINT('',(48.5,8.95,8.));
#11713=CARTESIAN_POINT('',(48.5,8.95,8.));
#11714=CARTESIAN_POINT('Origin',(50.,8.95,8.));
#11715=CARTESIAN_POINT('Origin',(50.,8.95,8.));
#11716=CARTESIAN_POINT('',(48.9,8.95,8.));
#11717=CARTESIAN_POINT('Origin',(50.,8.95,8.));
#11718=CARTESIAN_POINT('Origin',(50.,9.,8.));
#11719=CARTESIAN_POINT('',(48.9,9.2,8.));
#11720=CARTESIAN_POINT('Origin',(50.,9.2,8.));
#11721=CARTESIAN_POINT('',(48.9,9.,8.));
#11722=CARTESIAN_POINT('Origin',(50.,9.,8.));
#11723=CARTESIAN_POINT('',(48.,9.2,8.));
#11724=CARTESIAN_POINT('Origin',(50.,9.2,8.));
#11725=CARTESIAN_POINT('',(48.,9.,8.));
#11726=CARTESIAN_POINT('',(48.,9.,8.));
#11727=CARTESIAN_POINT('Origin',(50.,9.,8.));
#11728=CARTESIAN_POINT('Origin',(50.,9.2,8.));
#11729=CARTESIAN_POINT('Origin',(50.,9.,8.));
#11730=CARTESIAN_POINT('',(0.,0.,0.));
#11731=CARTESIAN_POINT('Origin',(1.,0.,0.4));
#11732=CARTESIAN_POINT('',(1.,0.36,0.7));
#11733=CARTESIAN_POINT('',(1.,0.4,0.66));
#11734=CARTESIAN_POINT('',(1.,0.355,0.705));
#11735=CARTESIAN_POINT('',(1.,-0.36,0.7));
#11736=CARTESIAN_POINT('',(1.,0.,0.7));
#11737=CARTESIAN_POINT('',(1.,-0.4,0.66));
#11738=CARTESIAN_POINT('',(1.,-0.355,0.705));
#11739=CARTESIAN_POINT('',(1.,-0.4,0.04));
#11740=CARTESIAN_POINT('',(1.,-0.4,0.2));
#11741=CARTESIAN_POINT('',(1.,-0.36,0.));
#11742=CARTESIAN_POINT('',(1.,-0.38,0.0199999999999999));
#11743=CARTESIAN_POINT('',(1.,0.36,0.));
#11744=CARTESIAN_POINT('',(1.,0.,0.));
#11745=CARTESIAN_POINT('',(1.,0.4,0.04));
#11746=CARTESIAN_POINT('',(1.,0.38,0.0199999999999999));
#11747=CARTESIAN_POINT('',(1.,0.4,0.2));
#11748=CARTESIAN_POINT('Origin',(-0.8,-0.38,0.02));
#11749=CARTESIAN_POINT('',(-1.,-0.4,0.04));
#11750=CARTESIAN_POINT('',(-0.8,-0.4,0.04));
#11751=CARTESIAN_POINT('',(-1.,-0.36,0.));
#11752=CARTESIAN_POINT('',(-1.,-0.38,0.0199999999999999));
#11753=CARTESIAN_POINT('',(-0.8,-0.36,0.));
#11754=CARTESIAN_POINT('Origin',(-1.6,-0.4,0.));
#11755=CARTESIAN_POINT('',(-1.,-0.4,0.66));
#11756=CARTESIAN_POINT('',(-0.8,-0.4,0.66));
#11757=CARTESIAN_POINT('',(-1.,-0.4,0.2));
#11758=CARTESIAN_POINT('Origin',(-0.8,-0.38,0.68));
#11759=CARTESIAN_POINT('',(-1.,-0.36,0.7));
#11760=CARTESIAN_POINT('',(-0.8,-0.36,0.7));
#11761=CARTESIAN_POINT('',(-1.,-0.355,0.705));
#11762=CARTESIAN_POINT('Origin',(0.,0.,0.7));
#11763=CARTESIAN_POINT('',(-1.,0.36,0.7));
#11764=CARTESIAN_POINT('',(0.8,0.36,0.7));
#11765=CARTESIAN_POINT('',(-1.,0.,0.7));
#11766=CARTESIAN_POINT('Origin',(-1.,0.,0.4));
#11767=CARTESIAN_POINT('',(-1.,0.4,0.66));
#11768=CARTESIAN_POINT('',(-1.,0.355,0.705));
#11769=CARTESIAN_POINT('',(-1.,0.4,0.04));
#11770=CARTESIAN_POINT('',(-1.,0.4,0.2));
#11771=CARTESIAN_POINT('',(-1.,0.36,0.));
#11772=CARTESIAN_POINT('',(-1.,0.38,0.0199999999999999));
#11773=CARTESIAN_POINT('',(-1.,0.,0.));
#11774=CARTESIAN_POINT('Origin',(0.8,0.38,0.68));
#11775=CARTESIAN_POINT('',(0.8,0.4,0.66));
#11776=CARTESIAN_POINT('Origin',(1.6,0.4,0.));
#11777=CARTESIAN_POINT('',(0.8,0.4,0.04));
#11778=CARTESIAN_POINT('Origin',(0.8,0.38,0.02));
#11779=CARTESIAN_POINT('',(0.8,0.36,0.));
#11780=CARTESIAN_POINT('Origin',(0.,0.,0.));
#11781=CARTESIAN_POINT('',(0.,0.,0.));
#11782=CARTESIAN_POINT('Origin',(0.0721687836487032,0.,-0.125));
#11783=CARTESIAN_POINT('',(0.0721687836487032,0.,-0.125));
#11784=CARTESIAN_POINT('',(0.144337567297406,0.,0.));
#11785=CARTESIAN_POINT('',(0.117710979560879,0.,-0.0461186027918559));
#11786=CARTESIAN_POINT('',(0.0721687836487032,-0.25,-0.125));
#11787=CARTESIAN_POINT('',(0.0721687836487032,0.,-0.125));
#11788=CARTESIAN_POINT('',(0.144337567297406,-0.25,0.));
#11789=CARTESIAN_POINT('',(0.144337567297406,-0.25,0.));
#11790=CARTESIAN_POINT('',(0.144337567297406,0.,0.));
#11791=CARTESIAN_POINT('Origin',(-0.0721687836487032,0.,-0.125));
#11792=CARTESIAN_POINT('',(-0.0721687836487032,0.,-0.125));
#11793=CARTESIAN_POINT('',(0.0739156081756484,0.,-0.125));
#11794=CARTESIAN_POINT('',(-0.0721687836487032,-0.25,-0.125));
#11795=CARTESIAN_POINT('',(-0.0721687836487032,0.,-0.125));
#11796=CARTESIAN_POINT('',(0.0721687836487032,-0.25,-0.125));
#11797=CARTESIAN_POINT('Origin',(-0.144337567297406,0.,-4.16333634234434E-17));
#11798=CARTESIAN_POINT('',(-0.144337567297406,0.,-1.76762539787485E-17));
#11799=CARTESIAN_POINT('',(-0.0987953713852306,0.,-0.0788813972081442));
#11800=CARTESIAN_POINT('',(-0.144337567297406,-0.25,-2.77555756156289E-17));
#11801=CARTESIAN_POINT('',(-0.144337567297406,0.,-1.76762539787485E-17));
#11802=CARTESIAN_POINT('',(-0.0721687836487032,-0.25,-0.125));
#11803=CARTESIAN_POINT('Origin',(-0.0721687836487033,0.,0.125));
#11804=CARTESIAN_POINT('',(-0.0721687836487033,0.,0.125));
#11805=CARTESIAN_POINT('',(-0.0627109795608791,0.,0.141381397208144));
#11806=CARTESIAN_POINT('',(-0.0721687836487033,-0.25,0.125));
#11807=CARTESIAN_POINT('',(-0.0721687836487033,0.,0.125));
#11808=CARTESIAN_POINT('',(-0.144337567297406,-0.25,-1.76762539787485E-17));
#11809=CARTESIAN_POINT('Origin',(0.0721687836487032,0.,0.125));
#11810=CARTESIAN_POINT('',(0.0721687836487032,0.,0.125));
#11811=CARTESIAN_POINT('',(0.146084391824352,0.,0.125));
#11812=CARTESIAN_POINT('',(0.0721687836487032,-0.25,0.125));
#11813=CARTESIAN_POINT('',(0.0721687836487032,0.,0.125));
#11814=CARTESIAN_POINT('',(-0.0721687836487033,-0.25,0.125));
#11815=CARTESIAN_POINT('Origin',(0.144337567297406,0.,0.));
#11816=CARTESIAN_POINT('',(0.153795371385231,0.,-0.0163813972081441));
#11817=CARTESIAN_POINT('',(0.0721687836487032,-0.25,0.125));
#11818=CARTESIAN_POINT('Origin',(0.,-0.25,0.));
#11819=CARTESIAN_POINT('Origin',(0.22,0.,0.));
#11820=CARTESIAN_POINT('',(-0.22,-8.67361737988404E-18,-2.69422295812418E-17));
#11821=CARTESIAN_POINT('Origin',(0.,0.,0.));
#11822=CARTESIAN_POINT('Origin',(0.,-0.015,0.));
#11823=CARTESIAN_POINT('',(-0.24505,-0.02505,-3.00099698131059E-17));
#11824=CARTESIAN_POINT('Origin',(0.,-0.02505,0.));
#11825=CARTESIAN_POINT('',(-0.235,-0.015,-2.87791997799628E-17));
#11826=CARTESIAN_POINT('Origin',(0.,-0.3775,0.));
#11827=CARTESIAN_POINT('',(-0.24505,-0.72995,3.00099698131059E-17));
#11828=CARTESIAN_POINT('Origin',(0.,-0.72995,0.));
#11829=CARTESIAN_POINT('',(-0.24505,-0.3775,-3.00099698131059E-17));
#11830=CARTESIAN_POINT('Origin',(0.,-0.7625,0.));
#11831=CARTESIAN_POINT('',(-0.175,-0.8,-2.14313189850787E-17));
#11832=CARTESIAN_POINT('Origin',(0.,-0.8,0.));
#11833=CARTESIAN_POINT('',(-0.2125,-0.7625,-2.60237444818813E-17));
#11834=CARTESIAN_POINT('Origin',(0.,-0.8,0.));
#11835=CARTESIAN_POINT('',(0.,0.,0.));
#11836=CARTESIAN_POINT('',(0.,0.,0.));
#11837=CARTESIAN_POINT('Origin',(0.,0.,0.));
#11838=CARTESIAN_POINT('',(-0.976185,-0.246528389340863,-1.19548183562566E-16));
#11839=CARTESIAN_POINT('',(-1.19548183562566E-16,-0.246528389340863,0.976185));
#11840=CARTESIAN_POINT('Origin',(0.,-0.246528389340863,0.));
#11841=CARTESIAN_POINT('Origin',(0.,-0.246528389340863,0.));
#11842=CARTESIAN_POINT('',(-1.19548183562566E-16,0.246528389340863,0.976185));
#11843=CARTESIAN_POINT('Origin',(-1.22464679914735E-16,0.,1.));
#11844=CARTESIAN_POINT('',(-0.976185,0.246528389340863,1.19548183562566E-16));
#11845=CARTESIAN_POINT('Origin',(0.,0.246528389340863,0.));
#11846=CARTESIAN_POINT('Origin',(0.,0.246528389340863,0.));
#11847=CARTESIAN_POINT('Origin',(0.,0.,0.));
#11848=CARTESIAN_POINT('',(-0.976185,0.45,-1.19548183562566E-16));
#11849=CARTESIAN_POINT('',(-0.976185,0.,-1.19548183562566E-16));
#11850=CARTESIAN_POINT('Origin',(0.,0.45,0.));
#11851=CARTESIAN_POINT('Origin',(0.,0.,0.));
#11852=CARTESIAN_POINT('',(-0.5,-0.39,-6.12323399573677E-17));
#11853=CARTESIAN_POINT('Origin',(0.,-0.39,0.));
#11854=CARTESIAN_POINT('',(-0.5,0.39,-6.12323399573677E-17));
#11855=CARTESIAN_POINT('',(-0.5,0.,-6.12323399573677E-17));
#11856=CARTESIAN_POINT('Origin',(0.,0.39,0.));
#11857=CARTESIAN_POINT('Origin',(0.,0.42,0.));
#11858=CARTESIAN_POINT('',(-0.56,0.45,-6.85802207522518E-17));
#11859=CARTESIAN_POINT('',(-0.53,0.42,-6.49062803548097E-17));
#11860=CARTESIAN_POINT('Origin',(0.,0.45,0.));
#11861=CARTESIAN_POINT('Origin',(0.976185,0.45,0.));
#11862=CARTESIAN_POINT('Origin',(0.,0.,0.));
#11863=CARTESIAN_POINT('',(-0.976185,-0.45,-1.19548183562566E-16));
#11864=CARTESIAN_POINT('Origin',(0.,-0.45,0.));
#11865=CARTESIAN_POINT('',(-0.976185,0.,-1.19548183562566E-16));
#11866=CARTESIAN_POINT('Origin',(0.56,-0.45,0.));
#11867=CARTESIAN_POINT('',(-0.56,-0.45,-6.85802207522518E-17));
#11868=CARTESIAN_POINT('Origin',(0.,-0.45,0.));
#11869=CARTESIAN_POINT('Origin',(0.,-0.42,0.));
#11870=CARTESIAN_POINT('',(-0.53,-0.42,-6.49062803548097E-17));
#11871=CARTESIAN_POINT('',(0.,0.,0.));
#11872=CARTESIAN_POINT('Origin',(0.,0.,0.));
#11873=CARTESIAN_POINT('',(-1.023815,0.246528389340863,-1.25381176266905E-16));
#11874=CARTESIAN_POINT('',(-1.25381176266905E-16,0.246528389340863,1.023815));
#11875=CARTESIAN_POINT('Origin',(0.,0.246528389340863,0.));
#11876=CARTESIAN_POINT('Origin',(0.,0.246528389340863,0.));
#11877=CARTESIAN_POINT('',(-1.25381176266905E-16,-0.246528389340863,1.023815));
#11878=CARTESIAN_POINT('Origin',(-1.22464679914735E-16,0.,1.));
#11879=CARTESIAN_POINT('',(-1.023815,-0.246528389340863,1.25381176266905E-16));
#11880=CARTESIAN_POINT('Origin',(0.,-0.246528389340863,0.));
#11881=CARTESIAN_POINT('Origin',(0.,-0.246528389340863,0.));
#11882=CARTESIAN_POINT('Origin',(0.,0.,0.));
#11883=CARTESIAN_POINT('',(-1.023815,-0.45,-1.25381176266905E-16));
#11884=CARTESIAN_POINT('Origin',(0.,-0.45,0.));
#11885=CARTESIAN_POINT('',(-1.023815,0.,-1.25381176266905E-16));
#11886=CARTESIAN_POINT('Origin',(1.44,0.45,0.));
#11887=CARTESIAN_POINT('',(-1.44,0.45,-1.76349139077219E-16));
#11888=CARTESIAN_POINT('Origin',(0.,0.45,0.));
#11889=CARTESIAN_POINT('',(-1.023815,0.45,-1.25381176266905E-16));
#11890=CARTESIAN_POINT('Origin',(0.,0.45,0.));
#11891=CARTESIAN_POINT('Origin',(0.,0.42,0.));
#11892=CARTESIAN_POINT('',(-1.5,0.39,-1.83697019872103E-16));
#11893=CARTESIAN_POINT('Origin',(0.,0.39,0.));
#11894=CARTESIAN_POINT('',(-1.47,0.42,-1.80023079474661E-16));
#11895=CARTESIAN_POINT('Origin',(0.,0.,0.));
#11896=CARTESIAN_POINT('',(-1.5,-0.39,-1.83697019872103E-16));
#11897=CARTESIAN_POINT('Origin',(0.,-0.39,0.));
#11898=CARTESIAN_POINT('',(-1.5,0.,-1.83697019872103E-16));
#11899=CARTESIAN_POINT('Origin',(0.,-0.42,0.));
#11900=CARTESIAN_POINT('',(-1.44,-0.45,-1.76349139077219E-16));
#11901=CARTESIAN_POINT('Origin',(0.,-0.45,0.));
#11902=CARTESIAN_POINT('',(-1.47,-0.42,-1.80023079474661E-16));
#11903=CARTESIAN_POINT('Origin',(1.023815,-0.45,0.));
#11904=CARTESIAN_POINT('Origin',(0.,0.,0.));
#11905=CARTESIAN_POINT('',(-1.023815,0.,-1.25381176266905E-16));
#11906=CARTESIAN_POINT('',(0.,0.,0.));
#11907=CARTESIAN_POINT('Origin',(1.,0.,0.));
#11908=CARTESIAN_POINT('',(1.,-1.78583896120461E-33,0.23815));
#11909=CARTESIAN_POINT('',(1.,-1.78583896120461E-33,-0.23815));
#11910=CARTESIAN_POINT('Origin',(1.,0.,0.));
#11911=CARTESIAN_POINT('Origin',(0.707106781186548,0.,-0.707106781186547));
#11912=CARTESIAN_POINT('',(0.875504261126124,-1.78583896120461E-33,-0.538709301246971));
#11913=CARTESIAN_POINT('',(0.538709301246971,-1.78583896120461E-33,-0.875504261126124));
#11914=CARTESIAN_POINT('Origin',(0.707106781186548,0.,-0.707106781186547));
#11915=CARTESIAN_POINT('Origin',(6.12323399573677E-17,0.,-1.));
#11916=CARTESIAN_POINT('',(0.23815,-1.78583896120461E-33,-1.));
#11917=CARTESIAN_POINT('',(-0.23815,-1.78583896120461E-33,-1.));
#11918=CARTESIAN_POINT('Origin',(6.12323399573677E-17,0.,-1.));
#11919=CARTESIAN_POINT('Origin',(-0.707106781186547,0.,-0.707106781186548));
#11920=CARTESIAN_POINT('',(-0.538709301246971,-1.78583896120461E-33,-0.875504261126124));
#11921=CARTESIAN_POINT('',(-0.875504261126124,-1.78583896120461E-33,-0.538709301246971));
#11922=CARTESIAN_POINT('Origin',(-0.707106781186547,0.,-0.707106781186548));
#11923=CARTESIAN_POINT('Origin',(-1.,0.,-1.22464679914735E-16));
#11924=CARTESIAN_POINT('',(-1.,-1.78583896120461E-33,-0.23815));
#11925=CARTESIAN_POINT('',(-1.,-1.78583896120461E-33,0.23815));
#11926=CARTESIAN_POINT('Origin',(-1.,0.,-1.22464679914735E-16));
#11927=CARTESIAN_POINT('Origin',(-0.707106781186548,0.,0.707106781186547));
#11928=CARTESIAN_POINT('',(-0.875504261126124,-7.94881478324376E-33,0.538709301246971));
#11929=CARTESIAN_POINT('',(-0.538709301246971,4.37713686083455E-33,0.875504261126124));
#11930=CARTESIAN_POINT('Origin',(-0.707106781186548,0.,0.707106781186547));
#11931=CARTESIAN_POINT('Origin',(-1.83697019872103E-16,0.,1.));
#11932=CARTESIAN_POINT('',(-0.23815,-1.78583896120461E-33,1.));
#11933=CARTESIAN_POINT('',(0.23815,-1.78583896120461E-33,1.));
#11934=CARTESIAN_POINT('Origin',(-1.83697019872103E-16,0.,1.));
#11935=CARTESIAN_POINT('Origin',(0.707106781186547,0.,0.707106781186548));
#11936=CARTESIAN_POINT('',(0.538709301246971,-4.86732687222419E-33,0.875504261126124));
#11937=CARTESIAN_POINT('',(0.875504261126124,1.29564894981497E-33,0.538709301246971));
#11938=CARTESIAN_POINT('Origin',(0.707106781186547,0.,0.707106781186548));
#11939=CARTESIAN_POINT('',(0.,0.,0.));
#11940=CARTESIAN_POINT('Origin',(0.707106781186547,0.,0.707106781186548));
#11941=CARTESIAN_POINT('',(0.504455939115715,-0.04763,0.841298510752802));
#11942=CARTESIAN_POINT('',(0.841298510752802,-0.04763,0.504455939115715));
#11943=CARTESIAN_POINT('Ctrl Pts',(0.504455939115715,-0.04763,0.841298510752802));
#11944=CARTESIAN_POINT('Ctrl Pts',(0.508899795931835,-0.0740444353928835,
0.838633903678357));
#11945=CARTESIAN_POINT('Ctrl Pts',(0.517157748491652,-0.0999305678883309,
0.833661031856294));
#11946=CARTESIAN_POINT('Ctrl Pts',(0.537715343527944,-0.142345102874864,
0.820511285096538));
#11947=CARTESIAN_POINT('Ctrl Pts',(0.548874290046456,-0.159766064500479,
0.813159949759));
#11948=CARTESIAN_POINT('Ctrl Pts',(0.573915184558107,-0.190326085855194,
0.795684265985089));
#11949=CARTESIAN_POINT('Ctrl Pts',(0.587792702767295,-0.203463743702801,
0.78555112003688));
#11950=CARTESIAN_POINT('Ctrl Pts',(0.615966552324775,-0.224161999508995,
0.763642258217233));
#11951=CARTESIAN_POINT('Ctrl Pts',(0.631684198665438,-0.232861760990032,
0.750785745543687));
#11952=CARTESIAN_POINT('Ctrl Pts',(0.663382628119203,-0.244251601209411,
0.722929908501543));
#11953=CARTESIAN_POINT('Ctrl Pts',(0.679352081686668,-0.246942143572133,
0.707917883896095));
#11954=CARTESIAN_POINT('Ctrl Pts',(0.707917883896095,-0.246942143572133,
0.679352081686668));
#11955=CARTESIAN_POINT('Ctrl Pts',(0.722929908501543,-0.244251601209411,
0.663382628119203));
#11956=CARTESIAN_POINT('Ctrl Pts',(0.750785745543687,-0.232861760990032,
0.631684198665439));
#11957=CARTESIAN_POINT('Ctrl Pts',(0.763642258217232,-0.224161999508995,
0.615966552324775));
#11958=CARTESIAN_POINT('Ctrl Pts',(0.78555112003688,-0.203463743702801,
0.587792702767295));
#11959=CARTESIAN_POINT('Ctrl Pts',(0.795684265985088,-0.190326085855194,
0.573915184558108));
#11960=CARTESIAN_POINT('Ctrl Pts',(0.813159949759,-0.15976606450048,0.548874290046456));
#11961=CARTESIAN_POINT('Ctrl Pts',(0.820511285096538,-0.142345102874864,
0.537715343527944));
#11962=CARTESIAN_POINT('Ctrl Pts',(0.833661031856294,-0.099930567888331,
0.517157748491653));
#11963=CARTESIAN_POINT('Ctrl Pts',(0.838633903678357,-0.0740444353928835,
0.508899795931835));
#11964=CARTESIAN_POINT('Ctrl Pts',(0.841298510752801,-0.0476299999999999,
0.504455939115715));
#11965=CARTESIAN_POINT('',(0.528110872004958,-0.04763,0.871530771444223));
#11966=CARTESIAN_POINT('Origin',(0.707106781186547,-0.04763,0.707106781186548));
#11967=CARTESIAN_POINT('',(0.871530771444223,-0.04763,0.528110872004959));
#11968=CARTESIAN_POINT('Ctrl Pts',(0.871530771444223,-0.0476300000000001,
0.528110872004958));
#11969=CARTESIAN_POINT('Ctrl Pts',(0.87014664509073,-0.0609922781173483,
0.530395067942936));
#11970=CARTESIAN_POINT('Ctrl Pts',(0.868149331745851,-0.0742967091364493,
0.533674141594226));
#11971=CARTESIAN_POINT('Ctrl Pts',(0.85981294420286,-0.115492077056649,
0.54708917182331));
#11972=CARTESIAN_POINT('Ctrl Pts',(0.850993704737257,-0.141695629206859,
0.560922177770136));
#11973=CARTESIAN_POINT('Ctrl Pts',(0.830754510485543,-0.181890537957859,
0.590422647829571));
#11974=CARTESIAN_POINT('Ctrl Pts',(0.816896541396381,-0.201072148666545,
0.609616703125488));
#11975=CARTESIAN_POINT('Ctrl Pts',(0.792310597819928,-0.223955109275652,
0.641117951819998));
#11976=CARTESIAN_POINT('Ctrl Pts',(0.779109323683612,-0.232742381310829,
0.657208095763053));
#11977=CARTESIAN_POINT('Ctrl Pts',(0.750552691816206,-0.244234834628584,
0.68964083160521));
#11978=CARTESIAN_POINT('Ctrl Pts',(0.735185187071673,-0.246942143572133,
0.705971972091755));
#11979=CARTESIAN_POINT('Ctrl Pts',(0.705971972091754,-0.246942143572133,
0.735185187071673));
#11980=CARTESIAN_POINT('Ctrl Pts',(0.689640831605209,-0.244234834628584,
0.750552691816206));
#11981=CARTESIAN_POINT('Ctrl Pts',(0.657208095763052,-0.232742381310829,
0.779109323683612));
#11982=CARTESIAN_POINT('Ctrl Pts',(0.641117951819998,-0.223955109275652,
0.792310597819928));
#11983=CARTESIAN_POINT('Ctrl Pts',(0.609616703125487,-0.201072148666545,
0.816896541396382));
#11984=CARTESIAN_POINT('Ctrl Pts',(0.590422647829571,-0.181890537957858,
0.830754510485544));
#11985=CARTESIAN_POINT('Ctrl Pts',(0.560922177770135,-0.141695629206858,
0.850993704737257));
#11986=CARTESIAN_POINT('Ctrl Pts',(0.547089171823309,-0.115492077056649,
0.859812944202861));
#11987=CARTESIAN_POINT('Ctrl Pts',(0.533674141594226,-0.0742967091364491,
0.868149331745852));
#11988=CARTESIAN_POINT('Ctrl Pts',(0.530395067942936,-0.0609922781173483,
0.870146645090731));
#11989=CARTESIAN_POINT('Ctrl Pts',(0.528110872004958,-0.0476300000000001,
0.871530771444223));
#11990=CARTESIAN_POINT('Origin',(0.707106781186547,-0.04763,0.707106781186548));
#11991=CARTESIAN_POINT('Origin',(0.,-0.166705,0.));
#11992=CARTESIAN_POINT('',(0.242834539687906,-0.04763,0.989696097314));
#11993=CARTESIAN_POINT('Origin',(0.,-0.04763,0.));
#11994=CARTESIAN_POINT('',(-0.242834539687907,-0.04763,0.989696097314));
#11995=CARTESIAN_POINT('Ctrl Pts',(0.242834539687906,-0.04763,0.989696097314));
#11996=CARTESIAN_POINT('Ctrl Pts',(0.24024064412003,-0.0609922781173483,
0.990332542620729));
#11997=CARTESIAN_POINT('Ctrl Pts',(0.236509675094874,-0.0742967091364492,
0.991238884025248));
#11998=CARTESIAN_POINT('Ctrl Pts',(0.221129100087819,-0.115492077056649,
0.994830026707808));
#11999=CARTESIAN_POINT('Ctrl Pts',(0.205111543747588,-0.141695629206859,
0.998375294985966));
#12000=CARTESIAN_POINT('Ctrl Pts',(0.169940289819232,-0.181890537957859,
1.00492400591205));
#12001=CARTESIAN_POINT('Ctrl Pts',(0.1465689792446,-0.201072148666545,1.00869718865384));
#12002=CARTESIAN_POINT('Ctrl Pts',(0.106909345252087,-0.223955109275652,
1.01358704779679));
#12003=CARTESIAN_POINT('Ctrl Pts',(0.0861971848975941,-0.232742381310829,
1.0156297872271));
#12004=CARTESIAN_POINT('Ctrl Pts',(0.0430711894098822,-0.244234834628584,
1.01837060663223));
#12005=CARTESIAN_POINT('Ctrl Pts',(0.0206568624125605,-0.246942143572133,
1.019052));
#12006=CARTESIAN_POINT('Ctrl Pts',(-0.0206568624125608,-0.246942143572133,
1.019052));
#12007=CARTESIAN_POINT('Ctrl Pts',(-0.0430711894098825,-0.244234834628584,
1.01837060663223));
#12008=CARTESIAN_POINT('Ctrl Pts',(-0.0861971848975943,-0.232742381310829,
1.0156297872271));
#12009=CARTESIAN_POINT('Ctrl Pts',(-0.106909345252088,-0.223955109275652,
1.01358704779679));
#12010=CARTESIAN_POINT('Ctrl Pts',(-0.1465689792446,-0.201072148666545,
1.00869718865384));
#12011=CARTESIAN_POINT('Ctrl Pts',(-0.169940289819232,-0.181890537957859,
1.00492400591205));
#12012=CARTESIAN_POINT('Ctrl Pts',(-0.205111543747588,-0.141695629206859,
0.998375294985966));
#12013=CARTESIAN_POINT('Ctrl Pts',(-0.221129100087819,-0.115492077056649,
0.994830026707808));
#12014=CARTESIAN_POINT('Ctrl Pts',(-0.236509675094875,-0.0742967091364493,
0.991238884025248));
#12015=CARTESIAN_POINT('Ctrl Pts',(-0.24024064412003,-0.0609922781173483,
0.990332542620729));
#12016=CARTESIAN_POINT('Ctrl Pts',(-0.242834539687907,-0.04763,0.989696097314));
#12017=CARTESIAN_POINT('',(-0.528110872004959,-0.04763,0.871530771444223));
#12018=CARTESIAN_POINT('Origin',(0.,-0.04763,0.));
#12019=CARTESIAN_POINT('',(-0.871530771444223,-0.04763,0.528110872004958));
#12020=CARTESIAN_POINT('Ctrl Pts',(-0.528110872004958,-0.0476300000000001,
0.871530771444223));
#12021=CARTESIAN_POINT('Ctrl Pts',(-0.530395067942936,-0.0609922781173484,
0.87014664509073));
#12022=CARTESIAN_POINT('Ctrl Pts',(-0.533674141594226,-0.0742967091364493,
0.868149331745851));
#12023=CARTESIAN_POINT('Ctrl Pts',(-0.54708917182331,-0.115492077056649,
0.85981294420286));
#12024=CARTESIAN_POINT('Ctrl Pts',(-0.560922177770136,-0.141695629206859,
0.850993704737257));
#12025=CARTESIAN_POINT('Ctrl Pts',(-0.590422647829571,-0.181890537957859,
0.830754510485543));
#12026=CARTESIAN_POINT('Ctrl Pts',(-0.609616703125488,-0.201072148666545,
0.816896541396381));
#12027=CARTESIAN_POINT('Ctrl Pts',(-0.641117951819998,-0.223955109275652,
0.792310597819928));
#12028=CARTESIAN_POINT('Ctrl Pts',(-0.657208095763053,-0.232742381310829,
0.779109323683611));
#12029=CARTESIAN_POINT('Ctrl Pts',(-0.68964083160521,-0.244234834628584,
0.750552691816205));
#12030=CARTESIAN_POINT('Ctrl Pts',(-0.705971972091755,-0.246942143572133,
0.735185187071673));
#12031=CARTESIAN_POINT('Ctrl Pts',(-0.735185187071673,-0.246942143572133,
0.705971972091754));
#12032=CARTESIAN_POINT('Ctrl Pts',(-0.750552691816206,-0.244234834628584,
0.689640831605209));
#12033=CARTESIAN_POINT('Ctrl Pts',(-0.779109323683612,-0.232742381310829,
0.657208095763052));
#12034=CARTESIAN_POINT('Ctrl Pts',(-0.792310597819928,-0.223955109275652,
0.641117951819998));
#12035=CARTESIAN_POINT('Ctrl Pts',(-0.816896541396382,-0.201072148666545,
0.609616703125487));
#12036=CARTESIAN_POINT('Ctrl Pts',(-0.830754510485544,-0.181890537957858,
0.590422647829571));
#12037=CARTESIAN_POINT('Ctrl Pts',(-0.850993704737257,-0.141695629206858,
0.560922177770135));
#12038=CARTESIAN_POINT('Ctrl Pts',(-0.859812944202861,-0.115492077056649,
0.547089171823309));
#12039=CARTESIAN_POINT('Ctrl Pts',(-0.868149331745852,-0.0742967091364491,
0.533674141594226));
#12040=CARTESIAN_POINT('Ctrl Pts',(-0.870146645090731,-0.0609922781173483,
0.530395067942936));
#12041=CARTESIAN_POINT('Ctrl Pts',(-0.871530771444223,-0.04763,0.528110872004958));
#12042=CARTESIAN_POINT('',(-0.989696097314,-0.04763,0.242834539687906));
#12043=CARTESIAN_POINT('Origin',(0.,-0.04763,0.));
#12044=CARTESIAN_POINT('',(-1.019052,-0.246942143572133,1.248489836334E-16));
#12045=CARTESIAN_POINT('Ctrl Pts',(-0.989696097314,-0.04763,0.242834539687906));
#12046=CARTESIAN_POINT('Ctrl Pts',(-0.990332542620729,-0.0609922781173483,
0.24024064412003));
#12047=CARTESIAN_POINT('Ctrl Pts',(-0.991238884025248,-0.0742967091364492,
0.236509675094874));
#12048=CARTESIAN_POINT('Ctrl Pts',(-0.994830026707808,-0.115492077056649,
0.221129100087819));
#12049=CARTESIAN_POINT('Ctrl Pts',(-0.998375294985966,-0.141695629206859,
0.205111543747588));
#12050=CARTESIAN_POINT('Ctrl Pts',(-1.00492400591205,-0.181890537957859,
0.169940289819232));
#12051=CARTESIAN_POINT('Ctrl Pts',(-1.00869718865384,-0.201072148666545,
0.1465689792446));
#12052=CARTESIAN_POINT('Ctrl Pts',(-1.01358704779679,-0.223955109275652,
0.106909345252088));
#12053=CARTESIAN_POINT('Ctrl Pts',(-1.0156297872271,-0.232742381310829,
0.0861971848975944));
#12054=CARTESIAN_POINT('Ctrl Pts',(-1.01837060663223,-0.244234834628584,
0.0430711894098825));
#12055=CARTESIAN_POINT('Ctrl Pts',(-1.019052,-0.246942143572133,0.0206568624125608));
#12056=CARTESIAN_POINT('Ctrl Pts',(-1.019052,-0.246942143572133,1.2490009027033E-16));
#12057=CARTESIAN_POINT('',(-1.019052,-0.28578,1.24797876996471E-16));
#12058=CARTESIAN_POINT('',(-1.019052,-0.166705,1.24797876996471E-16));
#12059=CARTESIAN_POINT('Origin',(0.,-0.28578,0.));
#12060=CARTESIAN_POINT('',(-0.989696097314,-0.04763,-0.242834539687906));
#12061=CARTESIAN_POINT('Ctrl Pts',(-1.019052,-0.246942143572133,1.2490009027033E-16));
#12062=CARTESIAN_POINT('Ctrl Pts',(-1.019052,-0.246942143572133,-0.0206568624125605));
#12063=CARTESIAN_POINT('Ctrl Pts',(-1.01837060663223,-0.244234834628584,
-0.0430711894098822));
#12064=CARTESIAN_POINT('Ctrl Pts',(-1.0156297872271,-0.232742381310829,
-0.0861971848975941));
#12065=CARTESIAN_POINT('Ctrl Pts',(-1.01358704779679,-0.223955109275652,
-0.106909345252087));
#12066=CARTESIAN_POINT('Ctrl Pts',(-1.00869718865384,-0.201072148666546,
-0.1465689792446));
#12067=CARTESIAN_POINT('Ctrl Pts',(-1.00492400591205,-0.181890537957859,
-0.169940289819232));
#12068=CARTESIAN_POINT('Ctrl Pts',(-0.998375294985966,-0.141695629206859,
-0.205111543747588));
#12069=CARTESIAN_POINT('Ctrl Pts',(-0.994830026707808,-0.11549207705665,
-0.221129100087819));
#12070=CARTESIAN_POINT('Ctrl Pts',(-0.991238884025248,-0.0742967091364495,
-0.236509675094874));
#12071=CARTESIAN_POINT('Ctrl Pts',(-0.990332542620729,-0.0609922781173484,
-0.24024064412003));
#12072=CARTESIAN_POINT('Ctrl Pts',(-0.989696097314,-0.0476300000000001,
-0.242834539687907));
#12073=CARTESIAN_POINT('',(-0.871530771444223,-0.04763,-0.528110872004958));
#12074=CARTESIAN_POINT('Origin',(0.,-0.04763,0.));
#12075=CARTESIAN_POINT('',(-0.528110872004958,-0.04763,-0.871530771444223));
#12076=CARTESIAN_POINT('Ctrl Pts',(-0.871530771444223,-0.0476300000000001,
-0.528110872004958));
#12077=CARTESIAN_POINT('Ctrl Pts',(-0.87014664509073,-0.0609922781173484,
-0.530395067942936));
#12078=CARTESIAN_POINT('Ctrl Pts',(-0.868149331745851,-0.0742967091364494,
-0.533674141594226));
#12079=CARTESIAN_POINT('Ctrl Pts',(-0.85981294420286,-0.115492077056649,
-0.54708917182331));
#12080=CARTESIAN_POINT('Ctrl Pts',(-0.850993704737257,-0.141695629206859,
-0.560922177770136));
#12081=CARTESIAN_POINT('Ctrl Pts',(-0.830754510485543,-0.181890537957859,
-0.590422647829571));
#12082=CARTESIAN_POINT('Ctrl Pts',(-0.816896541396381,-0.201072148666546,
-0.609616703125488));
#12083=CARTESIAN_POINT('Ctrl Pts',(-0.792310597819928,-0.223955109275652,
-0.641117951819999));
#12084=CARTESIAN_POINT('Ctrl Pts',(-0.779109323683611,-0.232742381310829,
-0.657208095763053));
#12085=CARTESIAN_POINT('Ctrl Pts',(-0.750552691816205,-0.244234834628584,
-0.68964083160521));
#12086=CARTESIAN_POINT('Ctrl Pts',(-0.735185187071673,-0.246942143572133,
-0.705971972091755));
#12087=CARTESIAN_POINT('Ctrl Pts',(-0.705971972091754,-0.246942143572133,
-0.735185187071673));
#12088=CARTESIAN_POINT('Ctrl Pts',(-0.68964083160521,-0.244234834628584,
-0.750552691816206));
#12089=CARTESIAN_POINT('Ctrl Pts',(-0.657208095763052,-0.232742381310829,
-0.779109323683612));
#12090=CARTESIAN_POINT('Ctrl Pts',(-0.641117951819998,-0.223955109275652,
-0.792310597819928));
#12091=CARTESIAN_POINT('Ctrl Pts',(-0.609616703125488,-0.201072148666545,
-0.816896541396381));
#12092=CARTESIAN_POINT('Ctrl Pts',(-0.590422647829571,-0.181890537957859,
-0.830754510485543));
#12093=CARTESIAN_POINT('Ctrl Pts',(-0.560922177770136,-0.141695629206859,
-0.850993704737257));
#12094=CARTESIAN_POINT('Ctrl Pts',(-0.54708917182331,-0.115492077056649,
-0.85981294420286));
#12095=CARTESIAN_POINT('Ctrl Pts',(-0.533674141594226,-0.0742967091364494,
-0.868149331745852));
#12096=CARTESIAN_POINT('Ctrl Pts',(-0.530395067942936,-0.0609922781173484,
-0.870146645090731));
#12097=CARTESIAN_POINT('Ctrl Pts',(-0.528110872004958,-0.0476300000000001,
-0.871530771444223));
#12098=CARTESIAN_POINT('',(-0.242834539687906,-0.04763,-0.989696097314));
#12099=CARTESIAN_POINT('Origin',(0.,-0.04763,0.));
#12100=CARTESIAN_POINT('',(0.242834539687906,-0.04763,-0.989696097314));
#12101=CARTESIAN_POINT('Ctrl Pts',(-0.242834539687907,-0.04763,-0.989696097314));
#12102=CARTESIAN_POINT('Ctrl Pts',(-0.24024064412003,-0.0609922781173483,
-0.990332542620729));
#12103=CARTESIAN_POINT('Ctrl Pts',(-0.236509675094874,-0.0742967091364493,
-0.991238884025248));
#12104=CARTESIAN_POINT('Ctrl Pts',(-0.221129100087819,-0.115492077056649,
-0.994830026707808));
#12105=CARTESIAN_POINT('Ctrl Pts',(-0.205111543747588,-0.141695629206859,
-0.998375294985966));
#12106=CARTESIAN_POINT('Ctrl Pts',(-0.169940289819232,-0.181890537957859,
-1.00492400591205));
#12107=CARTESIAN_POINT('Ctrl Pts',(-0.1465689792446,-0.201072148666545,
-1.00869718865384));
#12108=CARTESIAN_POINT('Ctrl Pts',(-0.106909345252087,-0.223955109275652,
-1.01358704779679));
#12109=CARTESIAN_POINT('Ctrl Pts',(-0.0861971848975942,-0.232742381310829,
-1.0156297872271));
#12110=CARTESIAN_POINT('Ctrl Pts',(-0.0430711894098823,-0.244234834628584,
-1.01837060663223));
#12111=CARTESIAN_POINT('Ctrl Pts',(-0.0206568624125606,-0.246942143572133,
-1.019052));
#12112=CARTESIAN_POINT('Ctrl Pts',(0.0206568624125607,-0.246942143572133,
-1.019052));
#12113=CARTESIAN_POINT('Ctrl Pts',(0.0430711894098824,-0.244234834628584,
-1.01837060663223));
#12114=CARTESIAN_POINT('Ctrl Pts',(0.0861971848975943,-0.232742381310829,
-1.0156297872271));
#12115=CARTESIAN_POINT('Ctrl Pts',(0.106909345252088,-0.223955109275652,
-1.01358704779679));
#12116=CARTESIAN_POINT('Ctrl Pts',(0.1465689792446,-0.201072148666545,-1.00869718865384));
#12117=CARTESIAN_POINT('Ctrl Pts',(0.169940289819232,-0.181890537957859,
-1.00492400591205));
#12118=CARTESIAN_POINT('Ctrl Pts',(0.205111543747588,-0.141695629206859,
-0.998375294985966));
#12119=CARTESIAN_POINT('Ctrl Pts',(0.221129100087819,-0.115492077056649,
-0.994830026707808));
#12120=CARTESIAN_POINT('Ctrl Pts',(0.236509675094874,-0.0742967091364493,
-0.991238884025248));
#12121=CARTESIAN_POINT('Ctrl Pts',(0.24024064412003,-0.0609922781173484,
-0.990332542620729));
#12122=CARTESIAN_POINT('Ctrl Pts',(0.242834539687907,-0.04763,-0.989696097314));
#12123=CARTESIAN_POINT('',(0.528110872004958,-0.04763,-0.871530771444223));
#12124=CARTESIAN_POINT('Origin',(0.,-0.04763,0.));
#12125=CARTESIAN_POINT('',(0.871530771444223,-0.04763,-0.528110872004958));
#12126=CARTESIAN_POINT('Ctrl Pts',(0.528110872004958,-0.0476300000000001,
-0.871530771444223));
#12127=CARTESIAN_POINT('Ctrl Pts',(0.530395067942936,-0.0609922781173484,
-0.870146645090731));
#12128=CARTESIAN_POINT('Ctrl Pts',(0.533674141594226,-0.0742967091364493,
-0.868149331745851));
#12129=CARTESIAN_POINT('Ctrl Pts',(0.54708917182331,-0.115492077056649,
-0.85981294420286));
#12130=CARTESIAN_POINT('Ctrl Pts',(0.560922177770136,-0.141695629206859,
-0.850993704737257));
#12131=CARTESIAN_POINT('Ctrl Pts',(0.590422647829571,-0.181890537957859,
-0.830754510485543));
#12132=CARTESIAN_POINT('Ctrl Pts',(0.609616703125488,-0.201072148666545,
-0.816896541396381));
#12133=CARTESIAN_POINT('Ctrl Pts',(0.641117951819998,-0.223955109275652,
-0.792310597819928));
#12134=CARTESIAN_POINT('Ctrl Pts',(0.657208095763053,-0.232742381310829,
-0.779109323683612));
#12135=CARTESIAN_POINT('Ctrl Pts',(0.68964083160521,-0.244234834628584,
-0.750552691816206));
#12136=CARTESIAN_POINT('Ctrl Pts',(0.705971972091755,-0.246942143572133,
-0.735185187071673));
#12137=CARTESIAN_POINT('Ctrl Pts',(0.735185187071673,-0.246942143572133,
-0.705971972091754));
#12138=CARTESIAN_POINT('Ctrl Pts',(0.750552691816206,-0.244234834628584,
-0.68964083160521));
#12139=CARTESIAN_POINT('Ctrl Pts',(0.779109323683612,-0.232742381310829,
-0.657208095763053));
#12140=CARTESIAN_POINT('Ctrl Pts',(0.792310597819928,-0.223955109275652,
-0.641117951819998));
#12141=CARTESIAN_POINT('Ctrl Pts',(0.816896541396381,-0.201072148666545,
-0.609616703125488));
#12142=CARTESIAN_POINT('Ctrl Pts',(0.830754510485543,-0.181890537957859,
-0.590422647829571));
#12143=CARTESIAN_POINT('Ctrl Pts',(0.850993704737257,-0.141695629206859,
-0.560922177770136));
#12144=CARTESIAN_POINT('Ctrl Pts',(0.85981294420286,-0.115492077056649,
-0.54708917182331));
#12145=CARTESIAN_POINT('Ctrl Pts',(0.868149331745851,-0.0742967091364493,
-0.533674141594226));
#12146=CARTESIAN_POINT('Ctrl Pts',(0.870146645090731,-0.0609922781173484,
-0.530395067942936));
#12147=CARTESIAN_POINT('Ctrl Pts',(0.871530771444223,-0.0476300000000001,
-0.528110872004958));
#12148=CARTESIAN_POINT('',(0.989696097314,-0.04763,-0.242834539687906));
#12149=CARTESIAN_POINT('Origin',(0.,-0.04763,0.));
#12150=CARTESIAN_POINT('',(0.989696097314,-0.04763,0.242834539687906));
#12151=CARTESIAN_POINT('Ctrl Pts',(0.989696097314,-0.04763,-0.242834539687907));
#12152=CARTESIAN_POINT('Ctrl Pts',(0.990332542620729,-0.0609922781173483,
-0.24024064412003));
#12153=CARTESIAN_POINT('Ctrl Pts',(0.991238884025248,-0.0742967091364493,
-0.236509675094874));
#12154=CARTESIAN_POINT('Ctrl Pts',(0.994830026707808,-0.115492077056649,
-0.221129100087819));
#12155=CARTESIAN_POINT('Ctrl Pts',(0.998375294985966,-0.141695629206859,
-0.205111543747588));
#12156=CARTESIAN_POINT('Ctrl Pts',(1.00492400591205,-0.181890537957859,
-0.169940289819232));
#12157=CARTESIAN_POINT('Ctrl Pts',(1.00869718865384,-0.201072148666545,
-0.1465689792446));
#12158=CARTESIAN_POINT('Ctrl Pts',(1.01358704779679,-0.223955109275652,
-0.106909345252087));
#12159=CARTESIAN_POINT('Ctrl Pts',(1.0156297872271,-0.232742381310829,-0.0861971848975942));
#12160=CARTESIAN_POINT('Ctrl Pts',(1.01837060663223,-0.244234834628584,
-0.0430711894098823));
#12161=CARTESIAN_POINT('Ctrl Pts',(1.019052,-0.246942143572133,-0.0206568624125607));
#12162=CARTESIAN_POINT('Ctrl Pts',(1.019052,-0.246942143572133,0.0206568624125607));
#12163=CARTESIAN_POINT('Ctrl Pts',(1.01837060663223,-0.244234834628584,
0.0430711894098823));
#12164=CARTESIAN_POINT('Ctrl Pts',(1.0156297872271,-0.232742381310829,0.0861971848975942));
#12165=CARTESIAN_POINT('Ctrl Pts',(1.01358704779679,-0.223955109275652,
0.106909345252087));
#12166=CARTESIAN_POINT('Ctrl Pts',(1.00869718865384,-0.201072148666545,
0.1465689792446));
#12167=CARTESIAN_POINT('Ctrl Pts',(1.00492400591205,-0.181890537957859,
0.169940289819232));
#12168=CARTESIAN_POINT('Ctrl Pts',(0.998375294985966,-0.141695629206859,
0.205111543747588));
#12169=CARTESIAN_POINT('Ctrl Pts',(0.994830026707808,-0.115492077056649,
0.221129100087819));
#12170=CARTESIAN_POINT('Ctrl Pts',(0.991238884025248,-0.0742967091364492,
0.236509675094874));
#12171=CARTESIAN_POINT('Ctrl Pts',(0.990332542620729,-0.0609922781173483,
0.24024064412003));
#12172=CARTESIAN_POINT('Ctrl Pts',(0.989696097314,-0.04763,0.242834539687907));
#12173=CARTESIAN_POINT('Origin',(0.,-0.04763,0.));
#12174=CARTESIAN_POINT('Origin',(0.,-0.04763,0.));
#12175=CARTESIAN_POINT('',(0.238183666596899,-0.04763,0.951592097314));
#12176=CARTESIAN_POINT('Origin',(0.,-0.04763,0.));
#12177=CARTESIAN_POINT('Origin',(-1.94289029309402E-16,-0.04763,1.));
#12178=CARTESIAN_POINT('Origin',(-1.94289029309402E-16,0.,1.));
#12179=CARTESIAN_POINT('',(-0.2381836665969,-0.04763,0.951592097314));
#12180=CARTESIAN_POINT('Ctrl Pts',(-0.238183666596899,-0.0476299999999999,
0.951592097314));
#12181=CARTESIAN_POINT('Ctrl Pts',(-0.233157223576062,-0.0740444353928835,
0.952850216871763));
#12182=CARTESIAN_POINT('Ctrl Pts',(-0.223801617934946,-0.0999305678883309,
0.955173119738174));
#12183=CARTESIAN_POINT('Ctrl Pts',(-0.199966927975188,-0.142345102874864,
0.960411259488514));
#12184=CARTESIAN_POINT('Ctrl Pts',(-0.1868781821531,-0.159766064500479,
0.963103647174702));
#12185=CARTESIAN_POINT('Ctrl Pts',(-0.15681442133453,-0.190326085855194,
0.968453058988463));
#12186=CARTESIAN_POINT('Ctrl Pts',(-0.139836317888043,-0.203463743702801,
0.971100730005489));
#12187=CARTESIAN_POINT('Ctrl Pts',(-0.104422493053067,-0.224161999508995,
0.975530745318961));
#12188=CARTESIAN_POINT('Ctrl Pts',(-0.0842175114474176,-0.232861760990032,
0.977553872336861));
#12189=CARTESIAN_POINT('Ctrl Pts',(-0.0421062857595701,-0.244251601209411,
0.980270995488453));
#12190=CARTESIAN_POINT('Ctrl Pts',(-0.0201990724523197,-0.246942143572133,
0.980948));
#12191=CARTESIAN_POINT('Ctrl Pts',(0.020199072452319,-0.246942143572133,
0.980948));
#12192=CARTESIAN_POINT('Ctrl Pts',(0.0421062857595694,-0.244251601209411,
0.980270995488454));
#12193=CARTESIAN_POINT('Ctrl Pts',(0.0842175114474169,-0.232861760990032,
0.977553872336861));
#12194=CARTESIAN_POINT('Ctrl Pts',(0.104422493053067,-0.224161999508995,
0.975530745318961));
#12195=CARTESIAN_POINT('Ctrl Pts',(0.139836317888042,-0.203463743702801,
0.971100730005489));
#12196=CARTESIAN_POINT('Ctrl Pts',(0.15681442133453,-0.190326085855194,
0.968453058988463));
#12197=CARTESIAN_POINT('Ctrl Pts',(0.1868781821531,-0.15976606450048,0.963103647174702));
#12198=CARTESIAN_POINT('Ctrl Pts',(0.199966927975188,-0.142345102874864,
0.960411259488514));
#12199=CARTESIAN_POINT('Ctrl Pts',(0.223801617934945,-0.0999305678883309,
0.955173119738174));
#12200=CARTESIAN_POINT('Ctrl Pts',(0.233157223576061,-0.0740444353928835,
0.952850216871763));
#12201=CARTESIAN_POINT('Ctrl Pts',(0.238183666596899,-0.0476299999999999,
0.951592097314));
#12202=CARTESIAN_POINT('Origin',(-1.94289029309402E-16,-0.04763,1.));
#12203=CARTESIAN_POINT('Origin',(0.,-0.04763,0.));
#12204=CARTESIAN_POINT('',(-0.504455939115715,-0.04763,0.841298510752802));
#12205=CARTESIAN_POINT('Origin',(0.,-0.04763,0.));
#12206=CARTESIAN_POINT('Origin',(-0.707106781186548,-0.04763,0.707106781186547));
#12207=CARTESIAN_POINT('Origin',(-0.707106781186548,0.,0.707106781186547));
#12208=CARTESIAN_POINT('',(-0.841298510752802,-0.04763,0.504455939115715));
#12209=CARTESIAN_POINT('Ctrl Pts',(-0.841298510752802,-0.04763,0.504455939115715));
#12210=CARTESIAN_POINT('Ctrl Pts',(-0.838633903678357,-0.0740444353928835,
0.508899795931835));
#12211=CARTESIAN_POINT('Ctrl Pts',(-0.833661031856294,-0.0999305678883309,
0.517157748491652));
#12212=CARTESIAN_POINT('Ctrl Pts',(-0.820511285096538,-0.142345102874864,
0.537715343527944));
#12213=CARTESIAN_POINT('Ctrl Pts',(-0.813159949759,-0.159766064500479,0.548874290046456));
#12214=CARTESIAN_POINT('Ctrl Pts',(-0.795684265985089,-0.190326085855194,
0.573915184558107));
#12215=CARTESIAN_POINT('Ctrl Pts',(-0.78555112003688,-0.203463743702801,
0.587792702767295));
#12216=CARTESIAN_POINT('Ctrl Pts',(-0.763642258217233,-0.224161999508995,
0.615966552324775));
#12217=CARTESIAN_POINT('Ctrl Pts',(-0.750785745543687,-0.232861760990032,
0.631684198665438));
#12218=CARTESIAN_POINT('Ctrl Pts',(-0.722929908501543,-0.244251601209411,
0.663382628119203));
#12219=CARTESIAN_POINT('Ctrl Pts',(-0.707917883896095,-0.246942143572133,
0.679352081686668));
#12220=CARTESIAN_POINT('Ctrl Pts',(-0.679352081686668,-0.246942143572133,
0.707917883896095));
#12221=CARTESIAN_POINT('Ctrl Pts',(-0.663382628119203,-0.244251601209411,
0.722929908501544));
#12222=CARTESIAN_POINT('Ctrl Pts',(-0.631684198665438,-0.232861760990031,
0.750785745543687));
#12223=CARTESIAN_POINT('Ctrl Pts',(-0.615966552324775,-0.224161999508995,
0.763642258217233));
#12224=CARTESIAN_POINT('Ctrl Pts',(-0.587792702767295,-0.203463743702801,
0.78555112003688));
#12225=CARTESIAN_POINT('Ctrl Pts',(-0.573915184558107,-0.190326085855194,
0.795684265985088));
#12226=CARTESIAN_POINT('Ctrl Pts',(-0.548874290046456,-0.159766064500479,
0.813159949759));
#12227=CARTESIAN_POINT('Ctrl Pts',(-0.537715343527944,-0.142345102874864,
0.820511285096538));
#12228=CARTESIAN_POINT('Ctrl Pts',(-0.517157748491652,-0.0999305678883309,
0.833661031856294));
#12229=CARTESIAN_POINT('Ctrl Pts',(-0.508899795931835,-0.0740444353928835,
0.838633903678357));
#12230=CARTESIAN_POINT('Ctrl Pts',(-0.504455939115716,-0.04763,0.841298510752801));
#12231=CARTESIAN_POINT('Origin',(-0.707106781186548,-0.04763,0.707106781186547));
#12232=CARTESIAN_POINT('Origin',(0.,-0.04763,0.));
#12233=CARTESIAN_POINT('',(-0.951592097314,-0.04763,0.238183666596899));
#12234=CARTESIAN_POINT('Origin',(0.,-0.04763,0.));
#12235=CARTESIAN_POINT('Origin',(-1.,-0.04763,-1.11022302462516E-16));
#12236=CARTESIAN_POINT('Origin',(-1.,0.,-1.11022302462516E-16));
#12237=CARTESIAN_POINT('',(-0.951592097314,-0.04763,-0.2381836665969));
#12238=CARTESIAN_POINT('',(-0.980948,-0.246942143572133,1.08514323328844E-18));
#12239=CARTESIAN_POINT('Ctrl Pts',(-0.951592097314,-0.04763,-0.238183666596899));
#12240=CARTESIAN_POINT('Ctrl Pts',(-0.952850216871763,-0.0740444353928835,
-0.233157223576062));
#12241=CARTESIAN_POINT('Ctrl Pts',(-0.955173119738174,-0.0999305678883309,
-0.223801617934946));
#12242=CARTESIAN_POINT('Ctrl Pts',(-0.960411259488514,-0.142345102874864,
-0.199966927975188));
#12243=CARTESIAN_POINT('Ctrl Pts',(-0.963103647174702,-0.159766064500479,
-0.1868781821531));
#12244=CARTESIAN_POINT('Ctrl Pts',(-0.968453058988463,-0.190326085855194,
-0.15681442133453));
#12245=CARTESIAN_POINT('Ctrl Pts',(-0.971100730005489,-0.203463743702801,
-0.139836317888043));
#12246=CARTESIAN_POINT('Ctrl Pts',(-0.975530745318961,-0.224161999508995,
-0.104422493053067));
#12247=CARTESIAN_POINT('Ctrl Pts',(-0.977553872336861,-0.232861760990032,
-0.0842175114474175));
#12248=CARTESIAN_POINT('Ctrl Pts',(-0.980270995488453,-0.244251601209411,
-0.0421062857595699));
#12249=CARTESIAN_POINT('Ctrl Pts',(-0.980948,-0.246942143572133,-0.0201990724523195));
#12250=CARTESIAN_POINT('Ctrl Pts',(-0.980948,-0.246942143572133,-1.17961196366423E-16));
#12251=CARTESIAN_POINT('Origin',(-1.,-0.04763,-1.11022302462516E-16));
#12252=CARTESIAN_POINT('Ctrl Pts',(-0.980948,-0.246942143572133,-1.17961196366423E-16));
#12253=CARTESIAN_POINT('Ctrl Pts',(-0.980948,-0.246942143572133,0.0201990724523192));
#12254=CARTESIAN_POINT('Ctrl Pts',(-0.980270995488453,-0.244251601209411,
0.0421062857595695));
#12255=CARTESIAN_POINT('Ctrl Pts',(-0.977553872336861,-0.232861760990032,
0.0842175114474169));
#12256=CARTESIAN_POINT('Ctrl Pts',(-0.975530745318961,-0.224161999508995,
0.104422493053066));
#12257=CARTESIAN_POINT('Ctrl Pts',(-0.971100730005489,-0.203463743702801,
0.139836317888042));
#12258=CARTESIAN_POINT('Ctrl Pts',(-0.968453058988463,-0.190326085855194,
0.15681442133453));
#12259=CARTESIAN_POINT('Ctrl Pts',(-0.963103647174702,-0.15976606450048,
0.1868781821531));
#12260=CARTESIAN_POINT('Ctrl Pts',(-0.960411259488514,-0.142345102874864,
0.199966927975188));
#12261=CARTESIAN_POINT('Ctrl Pts',(-0.955173119738174,-0.099930567888331,
0.223801617934945));
#12262=CARTESIAN_POINT('Ctrl Pts',(-0.952850216871763,-0.0740444353928835,
0.233157223576061));
#12263=CARTESIAN_POINT('Ctrl Pts',(-0.951592097314,-0.04763,0.238183666596899));
#12264=CARTESIAN_POINT('Origin',(0.,-0.04763,0.));
#12265=CARTESIAN_POINT('',(-0.841298510752802,-0.04763,-0.504455939115715));
#12266=CARTESIAN_POINT('Origin',(0.,-0.04763,0.));
#12267=CARTESIAN_POINT('Origin',(-0.707106781186547,-0.04763,-0.707106781186548));
#12268=CARTESIAN_POINT('Origin',(-0.707106781186547,0.,-0.707106781186548));
#12269=CARTESIAN_POINT('',(-0.504455939115715,-0.04763,-0.841298510752802));
#12270=CARTESIAN_POINT('Ctrl Pts',(-0.504455939115715,-0.04763,-0.841298510752802));
#12271=CARTESIAN_POINT('Ctrl Pts',(-0.508899795931835,-0.0740444353928835,
-0.838633903678357));
#12272=CARTESIAN_POINT('Ctrl Pts',(-0.517157748491652,-0.0999305678883309,
-0.833661031856294));
#12273=CARTESIAN_POINT('Ctrl Pts',(-0.537715343527944,-0.142345102874864,
-0.820511285096538));
#12274=CARTESIAN_POINT('Ctrl Pts',(-0.548874290046456,-0.159766064500479,
-0.813159949759));
#12275=CARTESIAN_POINT('Ctrl Pts',(-0.573915184558107,-0.190326085855194,
-0.795684265985089));
#12276=CARTESIAN_POINT('Ctrl Pts',(-0.587792702767295,-0.203463743702801,
-0.78555112003688));
#12277=CARTESIAN_POINT('Ctrl Pts',(-0.615966552324775,-0.224161999508995,
-0.763642258217233));
#12278=CARTESIAN_POINT('Ctrl Pts',(-0.631684198665438,-0.232861760990032,
-0.750785745543687));
#12279=CARTESIAN_POINT('Ctrl Pts',(-0.663382628119203,-0.244251601209411,
-0.722929908501543));
#12280=CARTESIAN_POINT('Ctrl Pts',(-0.679352081686668,-0.246942143572133,
-0.707917883896095));
#12281=CARTESIAN_POINT('Ctrl Pts',(-0.707917883896095,-0.246942143572133,
-0.679352081686668));
#12282=CARTESIAN_POINT('Ctrl Pts',(-0.722929908501543,-0.244251601209411,
-0.663382628119203));
#12283=CARTESIAN_POINT('Ctrl Pts',(-0.750785745543687,-0.232861760990032,
-0.631684198665439));
#12284=CARTESIAN_POINT('Ctrl Pts',(-0.763642258217232,-0.224161999508995,
-0.615966552324775));
#12285=CARTESIAN_POINT('Ctrl Pts',(-0.78555112003688,-0.203463743702801,
-0.587792702767295));
#12286=CARTESIAN_POINT('Ctrl Pts',(-0.795684265985088,-0.190326085855194,
-0.573915184558107));
#12287=CARTESIAN_POINT('Ctrl Pts',(-0.813159949759,-0.15976606450048,-0.548874290046456));
#12288=CARTESIAN_POINT('Ctrl Pts',(-0.820511285096538,-0.142345102874864,
-0.537715343527944));
#12289=CARTESIAN_POINT('Ctrl Pts',(-0.833661031856294,-0.0999305678883311,
-0.517157748491652));
#12290=CARTESIAN_POINT('Ctrl Pts',(-0.838633903678357,-0.0740444353928836,
-0.508899795931835));
#12291=CARTESIAN_POINT('Ctrl Pts',(-0.841298510752801,-0.04763,-0.504455939115715));
#12292=CARTESIAN_POINT('Origin',(-0.707106781186547,-0.04763,-0.707106781186548));
#12293=CARTESIAN_POINT('Origin',(0.,-0.04763,0.));
#12294=CARTESIAN_POINT('',(-0.238183666596899,-0.04763,-0.951592097314));
#12295=CARTESIAN_POINT('Origin',(0.,-0.04763,0.));
#12296=CARTESIAN_POINT('Origin',(5.55111512312578E-17,-0.04763,-1.));
#12297=CARTESIAN_POINT('Origin',(5.55111512312578E-17,0.,-1.));
#12298=CARTESIAN_POINT('',(0.238183666596899,-0.04763,-0.951592097314));
#12299=CARTESIAN_POINT('Ctrl Pts',(0.238183666596899,-0.04763,-0.951592097314));
#12300=CARTESIAN_POINT('Ctrl Pts',(0.233157223576062,-0.0740444353928835,
-0.952850216871763));
#12301=CARTESIAN_POINT('Ctrl Pts',(0.223801617934946,-0.099930567888331,
-0.955173119738174));
#12302=CARTESIAN_POINT('Ctrl Pts',(0.199966927975188,-0.142345102874864,
-0.960411259488514));
#12303=CARTESIAN_POINT('Ctrl Pts',(0.1868781821531,-0.15976606450048,-0.963103647174702));
#12304=CARTESIAN_POINT('Ctrl Pts',(0.15681442133453,-0.190326085855194,
-0.968453058988463));
#12305=CARTESIAN_POINT('Ctrl Pts',(0.139836317888042,-0.203463743702801,
-0.971100730005489));
#12306=CARTESIAN_POINT('Ctrl Pts',(0.104422493053067,-0.224161999508995,
-0.975530745318961));
#12307=CARTESIAN_POINT('Ctrl Pts',(0.0842175114474173,-0.232861760990032,
-0.977553872336861));
#12308=CARTESIAN_POINT('Ctrl Pts',(0.0421062857595698,-0.244251601209411,
-0.980270995488453));
#12309=CARTESIAN_POINT('Ctrl Pts',(0.0201990724523194,-0.246942143572133,
-0.980948));
#12310=CARTESIAN_POINT('Ctrl Pts',(-0.0201990724523193,-0.246942143572133,
-0.980948));
#12311=CARTESIAN_POINT('Ctrl Pts',(-0.0421062857595697,-0.244251601209411,
-0.980270995488453));
#12312=CARTESIAN_POINT('Ctrl Pts',(-0.0842175114474171,-0.232861760990032,
-0.977553872336861));
#12313=CARTESIAN_POINT('Ctrl Pts',(-0.104422493053067,-0.224161999508995,
-0.975530745318961));
#12314=CARTESIAN_POINT('Ctrl Pts',(-0.139836317888042,-0.203463743702801,
-0.971100730005489));
#12315=CARTESIAN_POINT('Ctrl Pts',(-0.15681442133453,-0.190326085855194,
-0.968453058988463));
#12316=CARTESIAN_POINT('Ctrl Pts',(-0.1868781821531,-0.15976606450048,-0.963103647174702));
#12317=CARTESIAN_POINT('Ctrl Pts',(-0.199966927975188,-0.142345102874864,
-0.960411259488514));
#12318=CARTESIAN_POINT('Ctrl Pts',(-0.223801617934945,-0.099930567888331,
-0.955173119738174));
#12319=CARTESIAN_POINT('Ctrl Pts',(-0.233157223576062,-0.0740444353928835,
-0.952850216871763));
#12320=CARTESIAN_POINT('Ctrl Pts',(-0.238183666596899,-0.0476299999999999,
-0.951592097314));
#12321=CARTESIAN_POINT('Origin',(5.55111512312578E-17,-0.04763,-1.));
#12322=CARTESIAN_POINT('Origin',(0.,-0.04763,0.));
#12323=CARTESIAN_POINT('',(0.504455939115715,-0.04763,-0.841298510752802));
#12324=CARTESIAN_POINT('Origin',(0.,-0.04763,0.));
#12325=CARTESIAN_POINT('Origin',(0.707106781186548,-0.04763,-0.707106781186547));
#12326=CARTESIAN_POINT('Origin',(0.707106781186548,0.,-0.707106781186547));
#12327=CARTESIAN_POINT('',(0.841298510752802,-0.04763,-0.504455939115715));
#12328=CARTESIAN_POINT('Ctrl Pts',(0.841298510752802,-0.04763,-0.504455939115715));
#12329=CARTESIAN_POINT('Ctrl Pts',(0.838633903678357,-0.0740444353928835,
-0.508899795931835));
#12330=CARTESIAN_POINT('Ctrl Pts',(0.833661031856294,-0.0999305678883309,
-0.517157748491652));
#12331=CARTESIAN_POINT('Ctrl Pts',(0.820511285096538,-0.142345102874864,
-0.537715343527944));
#12332=CARTESIAN_POINT('Ctrl Pts',(0.813159949759,-0.159766064500479,-0.548874290046456));
#12333=CARTESIAN_POINT('Ctrl Pts',(0.795684265985088,-0.190326085855194,
-0.573915184558107));
#12334=CARTESIAN_POINT('Ctrl Pts',(0.78555112003688,-0.203463743702801,
-0.587792702767295));
#12335=CARTESIAN_POINT('Ctrl Pts',(0.763642258217233,-0.224161999508995,
-0.615966552324775));
#12336=CARTESIAN_POINT('Ctrl Pts',(0.750785745543687,-0.232861760990032,
-0.631684198665438));
#12337=CARTESIAN_POINT('Ctrl Pts',(0.722929908501543,-0.244251601209411,
-0.663382628119203));
#12338=CARTESIAN_POINT('Ctrl Pts',(0.707917883896095,-0.246942143572133,
-0.679352081686668));
#12339=CARTESIAN_POINT('Ctrl Pts',(0.679352081686668,-0.246942143572133,
-0.707917883896095));
#12340=CARTESIAN_POINT('Ctrl Pts',(0.663382628119203,-0.244251601209411,
-0.722929908501543));
#12341=CARTESIAN_POINT('Ctrl Pts',(0.631684198665438,-0.232861760990032,
-0.750785745543687));
#12342=CARTESIAN_POINT('Ctrl Pts',(0.615966552324775,-0.224161999508995,
-0.763642258217232));
#12343=CARTESIAN_POINT('Ctrl Pts',(0.587792702767295,-0.203463743702801,
-0.78555112003688));
#12344=CARTESIAN_POINT('Ctrl Pts',(0.573915184558107,-0.190326085855194,
-0.795684265985088));
#12345=CARTESIAN_POINT('Ctrl Pts',(0.548874290046456,-0.159766064500479,
-0.813159949759));
#12346=CARTESIAN_POINT('Ctrl Pts',(0.537715343527944,-0.142345102874864,
-0.820511285096538));
#12347=CARTESIAN_POINT('Ctrl Pts',(0.517157748491652,-0.099930567888331,
-0.833661031856294));
#12348=CARTESIAN_POINT('Ctrl Pts',(0.508899795931835,-0.0740444353928835,
-0.838633903678357));
#12349=CARTESIAN_POINT('Ctrl Pts',(0.504455939115715,-0.04763,-0.841298510752801));
#12350=CARTESIAN_POINT('Origin',(0.707106781186548,-0.04763,-0.707106781186547));
#12351=CARTESIAN_POINT('Origin',(0.,-0.166705,0.));
#12352=CARTESIAN_POINT('',(-0.980948,-0.28578,1.20131482833E-16));
#12353=CARTESIAN_POINT('Origin',(0.,-0.28578,0.));
#12354=CARTESIAN_POINT('',(-0.980948,-0.166705,1.20131482833E-16));
#12355=CARTESIAN_POINT('',(0.951592097314,-0.04763,0.238183666596899));
#12356=CARTESIAN_POINT('Origin',(0.,-0.04763,0.));
#12357=CARTESIAN_POINT('',(0.951592097314,-0.04763,-0.238183666596899));
#12358=CARTESIAN_POINT('Ctrl Pts',(0.951592097314,-0.04763,0.238183666596899));
#12359=CARTESIAN_POINT('Ctrl Pts',(0.952850216871763,-0.0740444353928835,
0.233157223576062));
#12360=CARTESIAN_POINT('Ctrl Pts',(0.955173119738174,-0.099930567888331,
0.223801617934945));
#12361=CARTESIAN_POINT('Ctrl Pts',(0.960411259488514,-0.142345102874864,
0.199966927975188));
#12362=CARTESIAN_POINT('Ctrl Pts',(0.963103647174702,-0.15976606450048,
0.1868781821531));
#12363=CARTESIAN_POINT('Ctrl Pts',(0.968453058988463,-0.190326085855194,
0.15681442133453));
#12364=CARTESIAN_POINT('Ctrl Pts',(0.971100730005489,-0.203463743702801,
0.139836317888042));
#12365=CARTESIAN_POINT('Ctrl Pts',(0.975530745318961,-0.224161999508995,
0.104422493053067));
#12366=CARTESIAN_POINT('Ctrl Pts',(0.977553872336861,-0.232861760990032,
0.0842175114474172));
#12367=CARTESIAN_POINT('Ctrl Pts',(0.980270995488453,-0.244251601209411,
0.0421062857595697));
#12368=CARTESIAN_POINT('Ctrl Pts',(0.980948,-0.246942143572133,0.0201990724523194));
#12369=CARTESIAN_POINT('Ctrl Pts',(0.980948,-0.246942143572133,-0.0201990724523194));
#12370=CARTESIAN_POINT('Ctrl Pts',(0.980270995488453,-0.244251601209411,
-0.0421062857595697));
#12371=CARTESIAN_POINT('Ctrl Pts',(0.977553872336861,-0.232861760990032,
-0.0842175114474172));
#12372=CARTESIAN_POINT('Ctrl Pts',(0.975530745318961,-0.224161999508995,
-0.104422493053067));
#12373=CARTESIAN_POINT('Ctrl Pts',(0.971100730005489,-0.203463743702801,
-0.139836317888042));
#12374=CARTESIAN_POINT('Ctrl Pts',(0.968453058988463,-0.190326085855194,
-0.15681442133453));
#12375=CARTESIAN_POINT('Ctrl Pts',(0.963103647174702,-0.15976606450048,
-0.1868781821531));
#12376=CARTESIAN_POINT('Ctrl Pts',(0.960411259488514,-0.142345102874864,
-0.199966927975188));
#12377=CARTESIAN_POINT('Ctrl Pts',(0.955173119738174,-0.099930567888331,
-0.223801617934945));
#12378=CARTESIAN_POINT('Ctrl Pts',(0.952850216871763,-0.0740444353928835,
-0.233157223576062));
#12379=CARTESIAN_POINT('Ctrl Pts',(0.951592097314,-0.0476299999999999,-0.238183666596899));
#12380=CARTESIAN_POINT('Origin',(0.,-0.04763,0.));
#12381=CARTESIAN_POINT('Origin',(0.,-0.04763,0.));
#12382=CARTESIAN_POINT('Origin',(1.,-0.04763,0.));
#12383=CARTESIAN_POINT('Origin',(1.,0.,0.));
#12384=CARTESIAN_POINT('Origin',(1.,-0.04763,0.));
#12385=CARTESIAN_POINT('Origin',(0.,-0.28578,0.));
#12386=CARTESIAN_POINT('Origin',(0.,-0.04763,0.));
#12387=CARTESIAN_POINT('',(0.,0.,0.));
#12388=CARTESIAN_POINT('Origin',(1.013815,0.445,0.));
#12389=CARTESIAN_POINT('',(-1.013815,0.445,-1.24156529467757E-16));
#12390=CARTESIAN_POINT('Origin',(0.,0.445,0.));
#12391=CARTESIAN_POINT('',(-0.991185,0.445,-1.21385153761287E-16));
#12392=CARTESIAN_POINT('Origin',(0.,0.445,0.));
#12393=CARTESIAN_POINT('Origin',(0.,0.4075,0.));
#12394=CARTESIAN_POINT('',(-1.013815,0.37,-1.24156529467757E-16));
#12395=CARTESIAN_POINT('Origin',(0.,0.37,0.));
#12396=CARTESIAN_POINT('',(-1.013815,0.4075,-1.24156529467757E-16));
#12397=CARTESIAN_POINT('Origin',(0.991185,0.37,0.));
#12398=CARTESIAN_POINT('',(-0.991185,0.37,-1.21385153761287E-16));
#12399=CARTESIAN_POINT('Origin',(0.,0.37,0.));
#12400=CARTESIAN_POINT('Origin',(0.,0.4075,0.));
#12401=CARTESIAN_POINT('',(-0.991185,0.4075,-1.21385153761287E-16));
#12402=CARTESIAN_POINT('Origin',(1.013815,-0.37,0.));
#12403=CARTESIAN_POINT('',(-1.013815,-0.37,-1.24156529467757E-16));
#12404=CARTESIAN_POINT('Origin',(0.,-0.37,0.));
#12405=CARTESIAN_POINT('',(-0.991185,-0.37,-1.21385153761287E-16));
#12406=CARTESIAN_POINT('Origin',(0.,-0.37,0.));
#12407=CARTESIAN_POINT('Origin',(0.,-0.4075,0.));
#12408=CARTESIAN_POINT('',(-1.013815,-0.445,-1.24156529467757E-16));
#12409=CARTESIAN_POINT('Origin',(0.,-0.445,0.));
#12410=CARTESIAN_POINT('',(-1.013815,-0.4075,-1.24156529467757E-16));
#12411=CARTESIAN_POINT('Origin',(0.991185,-0.445,0.));
#12412=CARTESIAN_POINT('',(-0.991185,-0.445,-1.21385153761287E-16));
#12413=CARTESIAN_POINT('Origin',(0.,-0.445,0.));
#12414=CARTESIAN_POINT('Origin',(0.,-0.4075,0.));
#12415=CARTESIAN_POINT('',(-0.991185,-0.4075,-1.21385153761287E-16));
#12416=CARTESIAN_POINT('',(0.,0.,0.));
#12417=CARTESIAN_POINT('',(0.,0.,0.));
#12418=CARTESIAN_POINT('',(0.,0.,0.));
#12419=CARTESIAN_POINT('',(0.,0.,0.));
#12420=CARTESIAN_POINT('',(0.,0.,0.));
#12421=CARTESIAN_POINT('',(0.,0.,0.));
#12422=CARTESIAN_POINT('',(0.,0.,0.));
#12423=CARTESIAN_POINT('',(0.,0.,0.));
#12424=CARTESIAN_POINT('',(0.,0.,0.));
#12425=CARTESIAN_POINT('',(0.,0.,0.));
#12426=CARTESIAN_POINT('',(0.,0.,0.));
#12427=CARTESIAN_POINT('',(0.,0.,0.));
#12428=CARTESIAN_POINT('',(0.,-2.2,7.15));
#12429=CARTESIAN_POINT('',(-1.53824696311399E-31,8.8,7.15));
#12430=CARTESIAN_POINT('',(0.,6.8,10.05));
#12431=CARTESIAN_POINT('',(0.,-2.2,10.05));
#12432=CARTESIAN_POINT('',(0.,8.8,10.05));
#12433=CARTESIAN_POINT('',(50.,8.5,8.));
#12434=CARTESIAN_POINT('',(0.,0.,0.));
#12435=CARTESIAN_POINT('',(0.,0.,0.));
#12436=CARTESIAN_POINT('Origin',(50.,8.5,-0.1));
#12437=CARTESIAN_POINT('',(49.67,8.5,0.));
#12438=CARTESIAN_POINT('Origin',(50.,8.5,0.));
#12439=CARTESIAN_POINT('',(49.67,8.5,0.5));
#12440=CARTESIAN_POINT('',(49.67,8.5,-0.1));
#12441=CARTESIAN_POINT('Origin',(50.,8.5,0.5));
#12442=CARTESIAN_POINT('Origin',(50.,6.7,8.));
#12443=CARTESIAN_POINT('',(49.495,6.8,8.));
#12444=CARTESIAN_POINT('Origin',(50.,6.8,8.));
#12445=CARTESIAN_POINT('',(49.495,7.3,8.));
#12446=CARTESIAN_POINT('',(49.495,6.7,8.));
#12447=CARTESIAN_POINT('Origin',(50.,7.3,8.));
#12448=CARTESIAN_POINT('Origin',(50.,6.7,8.));
#12449=CARTESIAN_POINT('',(49.495,9.7,8.));
#12450=CARTESIAN_POINT('Origin',(50.,9.7,8.));
#12451=CARTESIAN_POINT('',(49.495,10.2,8.));
#12452=CARTESIAN_POINT('',(49.495,6.7,8.));
#12453=CARTESIAN_POINT('Origin',(50.,10.2,8.));
#12454=CARTESIAN_POINT('Origin',(49.,7.3,0.5));
#12455=CARTESIAN_POINT('',(51.,7.3,0.5));
#12456=CARTESIAN_POINT('',(49.,7.3,0.5));
#12457=CARTESIAN_POINT('',(49.5,7.3,0.5));
#12458=CARTESIAN_POINT('',(51.,9.7,0.5));
#12459=CARTESIAN_POINT('',(51.,7.3,0.5));
#12460=CARTESIAN_POINT('',(49.,9.7,0.5));
#12461=CARTESIAN_POINT('',(49.5,9.7,0.5));
#12462=CARTESIAN_POINT('',(49.,7.3,0.5));
#12463=CARTESIAN_POINT('Origin',(49.,9.7,9.));
#12464=CARTESIAN_POINT('',(51.,9.7,9.));
#12465=CARTESIAN_POINT('',(49.,9.7,9.));
#12466=CARTESIAN_POINT('',(51.,9.7,9.));
#12467=CARTESIAN_POINT('',(51.,10.2,9.));
#12468=CARTESIAN_POINT('',(51.,9.7,9.));
#12469=CARTESIAN_POINT('',(49.,10.2,9.));
#12470=CARTESIAN_POINT('',(51.,10.2,9.));
#12471=CARTESIAN_POINT('',(49.,9.7,9.));
#12472=CARTESIAN_POINT('Origin',(50.,10.2,4.5));
#12473=CARTESIAN_POINT('',(51.,10.2,0.));
#12474=CARTESIAN_POINT('',(51.,10.2,0.));
#12475=CARTESIAN_POINT('',(49.,10.2,0.));
#12476=CARTESIAN_POINT('',(49.,10.2,0.));
#12477=CARTESIAN_POINT('',(49.,10.2,9.));
#12478=CARTESIAN_POINT('Origin',(50.,9.7,4.5));
#12479=CARTESIAN_POINT('',(51.,9.7,0.));
#12480=CARTESIAN_POINT('',(49.,9.7,9.));
#12481=CARTESIAN_POINT('Origin',(50.,7.3,4.5));
#12482=CARTESIAN_POINT('',(49.,7.3,9.));
#12483=CARTESIAN_POINT('',(49.,7.3,9.));
#12484=CARTESIAN_POINT('',(51.,7.3,9.));
#12485=CARTESIAN_POINT('',(51.,7.3,9.));
#12486=CARTESIAN_POINT('',(51.,7.3,0.));
#12487=CARTESIAN_POINT('Origin',(49.,6.8,0.));
#12488=CARTESIAN_POINT('',(49.,6.8,9.));
#12489=CARTESIAN_POINT('',(49.,6.8,0.));
#12490=CARTESIAN_POINT('',(49.,6.8,9.));
#12491=CARTESIAN_POINT('',(49.,6.8,9.));
#12492=CARTESIAN_POINT('',(49.,6.8,0.));
#12493=CARTESIAN_POINT('Origin',(51.,6.8,0.));
#12494=CARTESIAN_POINT('',(51.,6.8,0.));
#12495=CARTESIAN_POINT('',(49.,6.8,0.));
#12496=CARTESIAN_POINT('',(51.,6.8,0.));
#12497=CARTESIAN_POINT('Origin',(51.,6.8,9.));
#12498=CARTESIAN_POINT('',(51.,6.8,9.));
#12499=CARTESIAN_POINT('',(51.,6.8,0.));
#12500=CARTESIAN_POINT('',(51.,6.8,9.));
#12501=CARTESIAN_POINT('Origin',(49.,6.8,9.));
#12502=CARTESIAN_POINT('',(51.,6.8,9.));
#12503=CARTESIAN_POINT('Origin',(50.,6.8,4.5));
#12504=CARTESIAN_POINT('',(0.,0.,0.));
#12505=CARTESIAN_POINT('Origin',(50.,9.2,8.));
#12506=CARTESIAN_POINT('',(49.835,9.2,8.));
#12507=CARTESIAN_POINT('Origin',(50.,9.2,8.));
#12508=CARTESIAN_POINT('',(49.835,10.4,8.));
#12509=CARTESIAN_POINT('',(49.835,9.2,8.));
#12510=CARTESIAN_POINT('Origin',(50.,10.4,8.));
#12511=CARTESIAN_POINT('Origin',(50.,9.2,8.));
#12512=CARTESIAN_POINT('Origin',(50.,6.5,8.));
#12513=CARTESIAN_POINT('',(49.835,6.6,8.));
#12514=CARTESIAN_POINT('Origin',(50.,6.6,8.));
#12515=CARTESIAN_POINT('',(49.835,7.8,8.));
#12516=CARTESIAN_POINT('',(49.835,6.5,8.));
#12517=CARTESIAN_POINT('Origin',(50.,7.8,8.));
#12518=CARTESIAN_POINT('Origin',(50.,7.8,8.));
#12519=CARTESIAN_POINT('Origin',(50.,6.6,8.));
#12520=CARTESIAN_POINT('',(49.5,10.4,8.));
#12521=CARTESIAN_POINT('Origin',(50.,10.4,8.));
#12522=CARTESIAN_POINT('',(49.5,6.6,8.));
#12523=CARTESIAN_POINT('',(49.5,6.6,8.));
#12524=CARTESIAN_POINT('Origin',(50.,6.6,8.));
#12525=CARTESIAN_POINT('Origin',(50.,10.4,8.));
#12526=CARTESIAN_POINT('Origin',(50.,6.6,8.));
#12527=CARTESIAN_POINT('',(0.,0.,0.));
#12528=CARTESIAN_POINT('Origin',(50.,7.3,8.));
#12529=CARTESIAN_POINT('',(49.495,8.05,8.));
#12530=CARTESIAN_POINT('Origin',(50.,8.05,8.));
#12531=CARTESIAN_POINT('',(49.495,7.3,8.));
#12532=CARTESIAN_POINT('',(49.495,7.3,8.));
#12533=CARTESIAN_POINT('Origin',(50.,7.3,8.));
#12534=CARTESIAN_POINT('Origin',(50.,7.3,8.));
#12535=CARTESIAN_POINT('',(49.3,8.05,8.));
#12536=CARTESIAN_POINT('Origin',(50.,8.05,8.));
#12537=CARTESIAN_POINT('',(49.3,7.3,8.));
#12538=CARTESIAN_POINT('',(49.3,7.3,8.));
#12539=CARTESIAN_POINT('Origin',(50.,7.3,8.));
#12540=CARTESIAN_POINT('Origin',(50.,8.05,8.));
#12541=CARTESIAN_POINT('Origin',(50.,7.3,8.));
#12542=CARTESIAN_POINT('',(0.,0.,0.));
#12543=CARTESIAN_POINT('Origin',(50.,8.95,8.));
#12544=CARTESIAN_POINT('',(49.495,9.7,8.));
#12545=CARTESIAN_POINT('Origin',(50.,9.7,8.));
#12546=CARTESIAN_POINT('',(49.495,8.95,8.));
#12547=CARTESIAN_POINT('',(49.495,8.95,8.));
#12548=CARTESIAN_POINT('Origin',(50.,8.95,8.));
#12549=CARTESIAN_POINT('Origin',(50.,8.95,8.));
#12550=CARTESIAN_POINT('',(49.3,9.7,8.));
#12551=CARTESIAN_POINT('Origin',(50.,9.7,8.));
#12552=CARTESIAN_POINT('',(49.3,8.95,8.));
#12553=CARTESIAN_POINT('',(49.3,8.95,8.));
#12554=CARTESIAN_POINT('Origin',(50.,8.95,8.));
#12555=CARTESIAN_POINT('Origin',(50.,9.7,8.));
#12556=CARTESIAN_POINT('Origin',(50.,8.95,8.));
#12557=CARTESIAN_POINT('',(0.,0.,0.));
#12558=CARTESIAN_POINT('Origin',(50.,6.6,8.));
#12559=CARTESIAN_POINT('',(49.495,6.8,8.));
#12560=CARTESIAN_POINT('Origin',(50.,6.8,8.));
#12561=CARTESIAN_POINT('',(49.495,6.6,8.));
#12562=CARTESIAN_POINT('',(49.495,6.6,8.));
#12563=CARTESIAN_POINT('Origin',(50.,6.6,8.));
#12564=CARTESIAN_POINT('Origin',(50.,6.6,8.));
#12565=CARTESIAN_POINT('',(49.3,6.8,8.));
#12566=CARTESIAN_POINT('Origin',(50.,6.8,8.));
#12567=CARTESIAN_POINT('',(49.3,6.6,8.));
#12568=CARTESIAN_POINT('',(49.3,6.6,8.));
#12569=CARTESIAN_POINT('Origin',(50.,6.6,8.));
#12570=CARTESIAN_POINT('Origin',(50.,6.8,8.));
#12571=CARTESIAN_POINT('Origin',(50.,6.6,8.));
#12572=CARTESIAN_POINT('',(0.,0.,0.));
#12573=CARTESIAN_POINT('Origin',(50.,10.2,8.));
#12574=CARTESIAN_POINT('',(49.495,10.4,8.));
#12575=CARTESIAN_POINT('Origin',(50.,10.4,8.));
#12576=CARTESIAN_POINT('',(49.495,10.2,8.));
#12577=CARTESIAN_POINT('',(49.495,10.2,8.));
#12578=CARTESIAN_POINT('Origin',(50.,10.2,8.));
#12579=CARTESIAN_POINT('Origin',(50.,10.2,8.));
#12580=CARTESIAN_POINT('',(49.3,10.4,8.));
#12581=CARTESIAN_POINT('Origin',(50.,10.4,8.));
#12582=CARTESIAN_POINT('',(49.3,10.2,8.));
#12583=CARTESIAN_POINT('',(49.3,10.2,8.));
#12584=CARTESIAN_POINT('Origin',(50.,10.2,8.));
#12585=CARTESIAN_POINT('Origin',(50.,10.4,8.));
#12586=CARTESIAN_POINT('Origin',(50.,10.2,8.));
#12587=CARTESIAN_POINT('',(0.,0.,0.));
#12588=CARTESIAN_POINT('Origin',(50.,6.4,8.));
#12589=CARTESIAN_POINT('',(49.775,6.6,8.));
#12590=CARTESIAN_POINT('Origin',(50.,6.6,8.));
#12591=CARTESIAN_POINT('',(49.775,6.4,8.));
#12592=CARTESIAN_POINT('',(49.775,6.4,8.));
#12593=CARTESIAN_POINT('Origin',(50.,6.4,8.));
#12594=CARTESIAN_POINT('Origin',(50.,6.4,8.));
#12595=CARTESIAN_POINT('',(49.2,6.6,8.));
#12596=CARTESIAN_POINT('Origin',(50.,6.6,8.));
#12597=CARTESIAN_POINT('',(49.2,6.4,8.));
#12598=CARTESIAN_POINT('',(49.2,6.4,8.));
#12599=CARTESIAN_POINT('Origin',(50.,6.4,8.));
#12600=CARTESIAN_POINT('Origin',(50.,6.6,8.));
#12601=CARTESIAN_POINT('Origin',(50.,6.4,8.));
#12602=CARTESIAN_POINT('',(0.,0.,0.));
#12603=CARTESIAN_POINT('Origin',(50.,10.4,8.));
#12604=CARTESIAN_POINT('',(49.775,10.6,8.));
#12605=CARTESIAN_POINT('Origin',(50.,10.6,8.));
#12606=CARTESIAN_POINT('',(49.775,10.4,8.));
#12607=CARTESIAN_POINT('',(49.775,10.4,8.));
#12608=CARTESIAN_POINT('Origin',(50.,10.4,8.));
#12609=CARTESIAN_POINT('Origin',(50.,10.4,8.));
#12610=CARTESIAN_POINT('',(49.2,10.6,8.));
#12611=CARTESIAN_POINT('Origin',(50.,10.6,8.));
#12612=CARTESIAN_POINT('',(49.2,10.4,8.));
#12613=CARTESIAN_POINT('',(49.2,10.4,8.));
#12614=CARTESIAN_POINT('Origin',(50.,10.4,8.));
#12615=CARTESIAN_POINT('Origin',(50.,10.6,8.));
#12616=CARTESIAN_POINT('Origin',(50.,10.4,8.));
#12617=CARTESIAN_POINT('',(0.,0.,0.));
#12618=CARTESIAN_POINT('Origin',(0.0866025403784439,-0.4,-0.15));
#12619=CARTESIAN_POINT('',(0.173205080756888,-0.4,0.));
#12620=CARTESIAN_POINT('',(0.0866025403784439,-0.4,-0.15));
#12621=CARTESIAN_POINT('',(0.173205080756888,-0.4,0.));
#12622=CARTESIAN_POINT('',(0.0866025403784439,-0.64,-0.15));
#12623=CARTESIAN_POINT('',(0.0866025403784439,-0.4,-0.15));
#12624=CARTESIAN_POINT('',(0.173205080756888,-0.64,0.));
#12625=CARTESIAN_POINT('',(0.173205080756888,-0.64,0.));
#12626=CARTESIAN_POINT('',(0.173205080756888,-0.4,0.));
#12627=CARTESIAN_POINT('Origin',(-0.0866025403784438,-0.4,-0.15));
#12628=CARTESIAN_POINT('',(-0.0866025403784438,-0.4,-0.15));
#12629=CARTESIAN_POINT('',(0.0866025403784439,-0.4,-0.15));
#12630=CARTESIAN_POINT('',(-0.0866025403784438,-0.64,-0.15));
#12631=CARTESIAN_POINT('',(-0.0866025403784438,-0.4,-0.15));
#12632=CARTESIAN_POINT('',(0.0866025403784439,-0.64,-0.15));
#12633=CARTESIAN_POINT('Origin',(-0.173205080756888,-0.4,-2.77555756156289E-17));
#12634=CARTESIAN_POINT('',(-0.173205080756888,-0.4,-2.12115047744981E-17));
#12635=CARTESIAN_POINT('',(-0.0866025403784438,-0.4,-0.15));
#12636=CARTESIAN_POINT('',(-0.173205080756888,-0.64,-2.77555756156289E-17));
#12637=CARTESIAN_POINT('',(-0.173205080756888,-0.4,-2.12115047744981E-17));
#12638=CARTESIAN_POINT('',(-0.0866025403784438,-0.64,-0.15));
#12639=CARTESIAN_POINT('Origin',(-0.0866025403784439,-0.4,0.15));
#12640=CARTESIAN_POINT('',(-0.0866025403784439,-0.4,0.15));
#12641=CARTESIAN_POINT('',(-0.173205080756888,-0.4,-2.12115047744981E-17));
#12642=CARTESIAN_POINT('',(-0.0866025403784439,-0.64,0.15));
#12643=CARTESIAN_POINT('',(-0.0866025403784439,-0.4,0.15));
#12644=CARTESIAN_POINT('',(-0.173205080756888,-0.64,-2.12115047744981E-17));
#12645=CARTESIAN_POINT('Origin',(0.0866025403784439,-0.4,0.15));
#12646=CARTESIAN_POINT('',(0.0866025403784439,-0.4,0.15));
#12647=CARTESIAN_POINT('',(-0.0866025403784439,-0.4,0.15));
#12648=CARTESIAN_POINT('',(0.0866025403784439,-0.64,0.15));
#12649=CARTESIAN_POINT('',(0.0866025403784439,-0.4,0.15));
#12650=CARTESIAN_POINT('',(-0.0866025403784439,-0.64,0.15));
#12651=CARTESIAN_POINT('Origin',(0.173205080756888,-0.4,0.));
#12652=CARTESIAN_POINT('',(0.0866025403784439,-0.4,0.15));
#12653=CARTESIAN_POINT('',(0.0866025403784439,-0.64,0.15));
#12654=CARTESIAN_POINT('Origin',(0.,-0.4,-2.77555756156289E-17));
#12655=CARTESIAN_POINT('Origin',(0.,-0.64,-2.77555756156289E-17));
#12656=CARTESIAN_POINT('Origin',(0.,-1.,0.));
#12657=CARTESIAN_POINT('',(-0.1954,-1.,2.39295984553393E-17));
#12658=CARTESIAN_POINT('Origin',(0.,-1.,0.));
#12659=CARTESIAN_POINT('Origin',(0.3,0.4,0.));
#12660=CARTESIAN_POINT('',(-0.3,0.4,-3.67394039744206E-17));
#12661=CARTESIAN_POINT('Origin',(0.,0.4,0.));
#12662=CARTESIAN_POINT('Origin',(0.,0.375,0.));
#12663=CARTESIAN_POINT('',(-0.35,0.35,-4.28626379701573E-17));
#12664=CARTESIAN_POINT('Origin',(0.,0.35,0.));
#12665=CARTESIAN_POINT('',(-0.325,0.375,-3.9801020972289E-17));
#12666=CARTESIAN_POINT('Origin',(0.,0.19,0.));
#12667=CARTESIAN_POINT('',(-0.35,0.03,-4.28626379701574E-17));
#12668=CARTESIAN_POINT('Origin',(0.,0.03,0.));
#12669=CARTESIAN_POINT('',(-0.35,0.19,-4.28626379701574E-17));
#12670=CARTESIAN_POINT('Origin',(0.,0.0149999999999999,0.));
#12671=CARTESIAN_POINT('',(-0.32,-3.29597460435593E-17,-3.91886975727153E-17));
#12672=CARTESIAN_POINT('Origin',(0.,0.,0.));
#12673=CARTESIAN_POINT('',(-0.335,0.0149999999999999,-4.10256677714363E-17));
#12674=CARTESIAN_POINT('Origin',(0.22,0.,0.));
#12675=CARTESIAN_POINT('',(-0.22,-6.93889390390723E-18,-2.69422295812418E-17));
#12676=CARTESIAN_POINT('Origin',(0.,0.,0.));
#12677=CARTESIAN_POINT('Origin',(0.,-0.02,0.));
#12678=CARTESIAN_POINT('',(-0.1954,-0.0492,2.39295984553393E-17));
#12679=CARTESIAN_POINT('Origin',(0.,-0.0492,0.));
#12680=CARTESIAN_POINT('',(-0.21,-0.02,-2.57175827820944E-17));
#12681=CARTESIAN_POINT('Origin',(0.,-0.8,0.));
#12682=CARTESIAN_POINT('',(-0.1954,-0.8,-2.39295984553393E-17));
#12683=CARTESIAN_POINT('',(0.,0.,0.));
#12684=CARTESIAN_POINT('',(0.,0.,0.));
#12685=CARTESIAN_POINT('',(0.,0.,0.));
#12686=CARTESIAN_POINT('',(0.,0.,0.));
#12687=CARTESIAN_POINT('',(0.,0.,0.));
#12688=CARTESIAN_POINT('',(0.,0.,0.));
#12689=CARTESIAN_POINT('',(0.,0.,0.));
#12690=CARTESIAN_POINT('',(0.,0.,0.));
#12691=CARTESIAN_POINT('',(50.,6.4,8.));
#12692=CARTESIAN_POINT('',(50.,10.6,8.));
#12693=CARTESIAN_POINT('',(0.,0.,0.));
#12694=CARTESIAN_POINT('',(0.,0.,0.));
#12695=CARTESIAN_POINT('',(0.,0.,0.));
#12696=UNCERTAINTY_MEASURE_WITH_UNIT(LENGTH_MEASURE(0.001),#12784,
'DISTANCE_ACCURACY_VALUE',
'Maximum model space distance between geometric entities at asserted c
onnectivities');
#12697=UNCERTAINTY_MEASURE_WITH_UNIT(LENGTH_MEASURE(0.001),#12784,
'DISTANCE_ACCURACY_VALUE',
'Maximum model space distance between geometric entities at asserted c
onnectivities');
#12698=UNCERTAINTY_MEASURE_WITH_UNIT(LENGTH_MEASURE(0.001),#12784,
'DISTANCE_ACCURACY_VALUE',
'Maximum model space distance between geometric entities at asserted c
onnectivities');
#12699=UNCERTAINTY_MEASURE_WITH_UNIT(LENGTH_MEASURE(0.001),#12784,
'DISTANCE_ACCURACY_VALUE',
'Maximum model space distance between geometric entities at asserted c
onnectivities');
#12700=UNCERTAINTY_MEASURE_WITH_UNIT(LENGTH_MEASURE(0.001),#12784,
'DISTANCE_ACCURACY_VALUE',
'Maximum model space distance between geometric entities at asserted c
onnectivities');
#12701=UNCERTAINTY_MEASURE_WITH_UNIT(LENGTH_MEASURE(0.001),#12784,
'DISTANCE_ACCURACY_VALUE',
'Maximum model space distance between geometric entities at asserted c
onnectivities');
#12702=UNCERTAINTY_MEASURE_WITH_UNIT(LENGTH_MEASURE(0.001),#12784,
'DISTANCE_ACCURACY_VALUE',
'Maximum model space distance between geometric entities at asserted c
onnectivities');
#12703=UNCERTAINTY_MEASURE_WITH_UNIT(LENGTH_MEASURE(0.001),#12784,
'DISTANCE_ACCURACY_VALUE',
'Maximum model space distance between geometric entities at asserted c
onnectivities');
#12704=UNCERTAINTY_MEASURE_WITH_UNIT(LENGTH_MEASURE(0.001),#12784,
'DISTANCE_ACCURACY_VALUE',
'Maximum model space distance between geometric entities at asserted c
onnectivities');
#12705=UNCERTAINTY_MEASURE_WITH_UNIT(LENGTH_MEASURE(0.001),#12784,
'DISTANCE_ACCURACY_VALUE',
'Maximum model space distance between geometric entities at asserted c
onnectivities');
#12706=UNCERTAINTY_MEASURE_WITH_UNIT(LENGTH_MEASURE(0.001),#12784,
'DISTANCE_ACCURACY_VALUE',
'Maximum model space distance between geometric entities at asserted c
onnectivities');
#12707=UNCERTAINTY_MEASURE_WITH_UNIT(LENGTH_MEASURE(0.001),#12784,
'DISTANCE_ACCURACY_VALUE',
'Maximum model space distance between geometric entities at asserted c
onnectivities');
#12708=UNCERTAINTY_MEASURE_WITH_UNIT(LENGTH_MEASURE(0.001),#12784,
'DISTANCE_ACCURACY_VALUE',
'Maximum model space distance between geometric entities at asserted c
onnectivities');
#12709=UNCERTAINTY_MEASURE_WITH_UNIT(LENGTH_MEASURE(0.001),#12784,
'DISTANCE_ACCURACY_VALUE',
'Maximum model space distance between geometric entities at asserted c
onnectivities');
#12710=UNCERTAINTY_MEASURE_WITH_UNIT(LENGTH_MEASURE(0.001),#12784,
'DISTANCE_ACCURACY_VALUE',
'Maximum model space distance between geometric entities at asserted c
onnectivities');
#12711=UNCERTAINTY_MEASURE_WITH_UNIT(LENGTH_MEASURE(0.001),#12784,
'DISTANCE_ACCURACY_VALUE',
'Maximum model space distance between geometric entities at asserted c
onnectivities');
#12712=UNCERTAINTY_MEASURE_WITH_UNIT(LENGTH_MEASURE(0.001),#12784,
'DISTANCE_ACCURACY_VALUE',
'Maximum model space distance between geometric entities at asserted c
onnectivities');
#12713=UNCERTAINTY_MEASURE_WITH_UNIT(LENGTH_MEASURE(0.001),#12784,
'DISTANCE_ACCURACY_VALUE',
'Maximum model space distance between geometric entities at asserted c
onnectivities');
#12714=UNCERTAINTY_MEASURE_WITH_UNIT(LENGTH_MEASURE(0.001),#12784,
'DISTANCE_ACCURACY_VALUE',
'Maximum model space distance between geometric entities at asserted c
onnectivities');
#12715=UNCERTAINTY_MEASURE_WITH_UNIT(LENGTH_MEASURE(0.001),#12784,
'DISTANCE_ACCURACY_VALUE',
'Maximum model space distance between geometric entities at asserted c
onnectivities');
#12716=UNCERTAINTY_MEASURE_WITH_UNIT(LENGTH_MEASURE(0.001),#12784,
'DISTANCE_ACCURACY_VALUE',
'Maximum model space distance between geometric entities at asserted c
onnectivities');
#12717=UNCERTAINTY_MEASURE_WITH_UNIT(LENGTH_MEASURE(0.001),#12784,
'DISTANCE_ACCURACY_VALUE',
'Maximum model space distance between geometric entities at asserted c
onnectivities');
#12718=UNCERTAINTY_MEASURE_WITH_UNIT(LENGTH_MEASURE(0.001),#12784,
'DISTANCE_ACCURACY_VALUE',
'Maximum model space distance between geometric entities at asserted c
onnectivities');
#12719=UNCERTAINTY_MEASURE_WITH_UNIT(LENGTH_MEASURE(0.001),#12784,
'DISTANCE_ACCURACY_VALUE',
'Maximum model space distance between geometric entities at asserted c
onnectivities');
#12720=UNCERTAINTY_MEASURE_WITH_UNIT(LENGTH_MEASURE(0.001),#12784,
'DISTANCE_ACCURACY_VALUE',
'Maximum model space distance between geometric entities at asserted c
onnectivities');
#12721=UNCERTAINTY_MEASURE_WITH_UNIT(LENGTH_MEASURE(0.001),#12784,
'DISTANCE_ACCURACY_VALUE',
'Maximum model space distance between geometric entities at asserted c
onnectivities');
#12722=UNCERTAINTY_MEASURE_WITH_UNIT(LENGTH_MEASURE(0.001),#12784,
'DISTANCE_ACCURACY_VALUE',
'Maximum model space distance between geometric entities at asserted c
onnectivities');
#12723=UNCERTAINTY_MEASURE_WITH_UNIT(LENGTH_MEASURE(0.001),#12784,
'DISTANCE_ACCURACY_VALUE',
'Maximum model space distance between geometric entities at asserted c
onnectivities');
#12724=UNCERTAINTY_MEASURE_WITH_UNIT(LENGTH_MEASURE(0.001),#12784,
'DISTANCE_ACCURACY_VALUE',
'Maximum model space distance between geometric entities at asserted c
onnectivities');
#12725=UNCERTAINTY_MEASURE_WITH_UNIT(LENGTH_MEASURE(0.001),#12784,
'DISTANCE_ACCURACY_VALUE',
'Maximum model space distance between geometric entities at asserted c
onnectivities');
#12726=UNCERTAINTY_MEASURE_WITH_UNIT(LENGTH_MEASURE(0.001),#12784,
'DISTANCE_ACCURACY_VALUE',
'Maximum model space distance between geometric entities at asserted c
onnectivities');
#12727=UNCERTAINTY_MEASURE_WITH_UNIT(LENGTH_MEASURE(0.001),#12784,
'DISTANCE_ACCURACY_VALUE',
'Maximum model space distance between geometric entities at asserted c
onnectivities');
#12728=UNCERTAINTY_MEASURE_WITH_UNIT(LENGTH_MEASURE(0.001),#12784,
'DISTANCE_ACCURACY_VALUE',
'Maximum model space distance between geometric entities at asserted c
onnectivities');
#12729=UNCERTAINTY_MEASURE_WITH_UNIT(LENGTH_MEASURE(0.001),#12784,
'DISTANCE_ACCURACY_VALUE',
'Maximum model space distance between geometric entities at asserted c
onnectivities');
#12730=UNCERTAINTY_MEASURE_WITH_UNIT(LENGTH_MEASURE(0.001),#12784,
'DISTANCE_ACCURACY_VALUE',
'Maximum model space distance between geometric entities at asserted c
onnectivities');
#12731=UNCERTAINTY_MEASURE_WITH_UNIT(LENGTH_MEASURE(0.001),#12784,
'DISTANCE_ACCURACY_VALUE',
'Maximum model space distance between geometric entities at asserted c
onnectivities');
#12732=UNCERTAINTY_MEASURE_WITH_UNIT(LENGTH_MEASURE(0.001),#12784,
'DISTANCE_ACCURACY_VALUE',
'Maximum model space distance between geometric entities at asserted c
onnectivities');
#12733=UNCERTAINTY_MEASURE_WITH_UNIT(LENGTH_MEASURE(0.001),#12784,
'DISTANCE_ACCURACY_VALUE',
'Maximum model space distance between geometric entities at asserted c
onnectivities');
#12734=UNCERTAINTY_MEASURE_WITH_UNIT(LENGTH_MEASURE(0.001),#12784,
'DISTANCE_ACCURACY_VALUE',
'Maximum model space distance between geometric entities at asserted c
onnectivities');
#12735=UNCERTAINTY_MEASURE_WITH_UNIT(LENGTH_MEASURE(0.001),#12784,
'DISTANCE_ACCURACY_VALUE',
'Maximum model space distance between geometric entities at asserted c
onnectivities');
#12736=UNCERTAINTY_MEASURE_WITH_UNIT(LENGTH_MEASURE(0.001),#12784,
'DISTANCE_ACCURACY_VALUE',
'Maximum model space distance between geometric entities at asserted c
onnectivities');
#12737=UNCERTAINTY_MEASURE_WITH_UNIT(LENGTH_MEASURE(0.001),#12784,
'DISTANCE_ACCURACY_VALUE',
'Maximum model space distance between geometric entities at asserted c
onnectivities');
#12738=UNCERTAINTY_MEASURE_WITH_UNIT(LENGTH_MEASURE(0.001),#12784,
'DISTANCE_ACCURACY_VALUE',
'Maximum model space distance between geometric entities at asserted c
onnectivities');
#12739=UNCERTAINTY_MEASURE_WITH_UNIT(LENGTH_MEASURE(0.001),#12784,
'DISTANCE_ACCURACY_VALUE',
'Maximum model space distance between geometric entities at asserted c
onnectivities');
#12740=(
GEOMETRIC_REPRESENTATION_CONTEXT(3)
GLOBAL_UNCERTAINTY_ASSIGNED_CONTEXT((#12696))
GLOBAL_UNIT_ASSIGNED_CONTEXT((#12784,#12786,#12787))
REPRESENTATION_CONTEXT('','3D')
);
#12741=(
GEOMETRIC_REPRESENTATION_CONTEXT(3)
GLOBAL_UNCERTAINTY_ASSIGNED_CONTEXT((#12697))
GLOBAL_UNIT_ASSIGNED_CONTEXT((#12784,#12786,#12787))
REPRESENTATION_CONTEXT('','3D')
);
#12742=(
GEOMETRIC_REPRESENTATION_CONTEXT(3)
GLOBAL_UNCERTAINTY_ASSIGNED_CONTEXT((#12698))
GLOBAL_UNIT_ASSIGNED_CONTEXT((#12784,#12786,#12787))
REPRESENTATION_CONTEXT('','3D')
);
#12743=(
GEOMETRIC_REPRESENTATION_CONTEXT(3)
GLOBAL_UNCERTAINTY_ASSIGNED_CONTEXT((#12699))
GLOBAL_UNIT_ASSIGNED_CONTEXT((#12784,#12786,#12787))
REPRESENTATION_CONTEXT('','3D')
);
#12744=(
GEOMETRIC_REPRESENTATION_CONTEXT(3)
GLOBAL_UNCERTAINTY_ASSIGNED_CONTEXT((#12700))
GLOBAL_UNIT_ASSIGNED_CONTEXT((#12784,#12786,#12787))
REPRESENTATION_CONTEXT('','3D')
);
#12745=(
GEOMETRIC_REPRESENTATION_CONTEXT(3)
GLOBAL_UNCERTAINTY_ASSIGNED_CONTEXT((#12701))
GLOBAL_UNIT_ASSIGNED_CONTEXT((#12784,#12786,#12787))
REPRESENTATION_CONTEXT('','3D')
);
#12746=(
GEOMETRIC_REPRESENTATION_CONTEXT(3)
GLOBAL_UNCERTAINTY_ASSIGNED_CONTEXT((#12702))
GLOBAL_UNIT_ASSIGNED_CONTEXT((#12784,#12786,#12787))
REPRESENTATION_CONTEXT('','3D')
);
#12747=(
GEOMETRIC_REPRESENTATION_CONTEXT(3)
GLOBAL_UNCERTAINTY_ASSIGNED_CONTEXT((#12703))
GLOBAL_UNIT_ASSIGNED_CONTEXT((#12784,#12786,#12787))
REPRESENTATION_CONTEXT('','3D')
);
#12748=(
GEOMETRIC_REPRESENTATION_CONTEXT(3)
GLOBAL_UNCERTAINTY_ASSIGNED_CONTEXT((#12704))
GLOBAL_UNIT_ASSIGNED_CONTEXT((#12784,#12786,#12787))
REPRESENTATION_CONTEXT('','3D')
);
#12749=(
GEOMETRIC_REPRESENTATION_CONTEXT(3)
GLOBAL_UNCERTAINTY_ASSIGNED_CONTEXT((#12705))
GLOBAL_UNIT_ASSIGNED_CONTEXT((#12784,#12786,#12787))
REPRESENTATION_CONTEXT('','3D')
);
#12750=(
GEOMETRIC_REPRESENTATION_CONTEXT(3)
GLOBAL_UNCERTAINTY_ASSIGNED_CONTEXT((#12706))
GLOBAL_UNIT_ASSIGNED_CONTEXT((#12784,#12786,#12787))
REPRESENTATION_CONTEXT('','3D')
);
#12751=(
GEOMETRIC_REPRESENTATION_CONTEXT(3)
GLOBAL_UNCERTAINTY_ASSIGNED_CONTEXT((#12707))
GLOBAL_UNIT_ASSIGNED_CONTEXT((#12784,#12786,#12787))
REPRESENTATION_CONTEXT('','3D')
);
#12752=(
GEOMETRIC_REPRESENTATION_CONTEXT(3)
GLOBAL_UNCERTAINTY_ASSIGNED_CONTEXT((#12708))
GLOBAL_UNIT_ASSIGNED_CONTEXT((#12784,#12786,#12787))
REPRESENTATION_CONTEXT('','3D')
);
#12753=(
GEOMETRIC_REPRESENTATION_CONTEXT(3)
GLOBAL_UNCERTAINTY_ASSIGNED_CONTEXT((#12709))
GLOBAL_UNIT_ASSIGNED_CONTEXT((#12784,#12786,#12787))
REPRESENTATION_CONTEXT('','3D')
);
#12754=(
GEOMETRIC_REPRESENTATION_CONTEXT(3)
GLOBAL_UNCERTAINTY_ASSIGNED_CONTEXT((#12710))
GLOBAL_UNIT_ASSIGNED_CONTEXT((#12784,#12786,#12787))
REPRESENTATION_CONTEXT('','3D')
);
#12755=(
GEOMETRIC_REPRESENTATION_CONTEXT(3)
GLOBAL_UNCERTAINTY_ASSIGNED_CONTEXT((#12711))
GLOBAL_UNIT_ASSIGNED_CONTEXT((#12784,#12786,#12787))
REPRESENTATION_CONTEXT('','3D')
);
#12756=(
GEOMETRIC_REPRESENTATION_CONTEXT(3)
GLOBAL_UNCERTAINTY_ASSIGNED_CONTEXT((#12712))
GLOBAL_UNIT_ASSIGNED_CONTEXT((#12784,#12786,#12787))
REPRESENTATION_CONTEXT('','3D')
);
#12757=(
GEOMETRIC_REPRESENTATION_CONTEXT(3)
GLOBAL_UNCERTAINTY_ASSIGNED_CONTEXT((#12713))
GLOBAL_UNIT_ASSIGNED_CONTEXT((#12784,#12786,#12787))
REPRESENTATION_CONTEXT('','3D')
);
#12758=(
GEOMETRIC_REPRESENTATION_CONTEXT(3)
GLOBAL_UNCERTAINTY_ASSIGNED_CONTEXT((#12714))
GLOBAL_UNIT_ASSIGNED_CONTEXT((#12784,#12786,#12787))
REPRESENTATION_CONTEXT('','3D')
);
#12759=(
GEOMETRIC_REPRESENTATION_CONTEXT(3)
GLOBAL_UNCERTAINTY_ASSIGNED_CONTEXT((#12715))
GLOBAL_UNIT_ASSIGNED_CONTEXT((#12784,#12786,#12787))
REPRESENTATION_CONTEXT('','3D')
);
#12760=(
GEOMETRIC_REPRESENTATION_CONTEXT(3)
GLOBAL_UNCERTAINTY_ASSIGNED_CONTEXT((#12716))
GLOBAL_UNIT_ASSIGNED_CONTEXT((#12784,#12786,#12787))
REPRESENTATION_CONTEXT('','3D')
);
#12761=(
GEOMETRIC_REPRESENTATION_CONTEXT(3)
GLOBAL_UNCERTAINTY_ASSIGNED_CONTEXT((#12717))
GLOBAL_UNIT_ASSIGNED_CONTEXT((#12784,#12786,#12787))
REPRESENTATION_CONTEXT('','3D')
);
#12762=(
GEOMETRIC_REPRESENTATION_CONTEXT(3)
GLOBAL_UNCERTAINTY_ASSIGNED_CONTEXT((#12718))
GLOBAL_UNIT_ASSIGNED_CONTEXT((#12784,#12786,#12787))
REPRESENTATION_CONTEXT('','3D')
);
#12763=(
GEOMETRIC_REPRESENTATION_CONTEXT(3)
GLOBAL_UNCERTAINTY_ASSIGNED_CONTEXT((#12719))
GLOBAL_UNIT_ASSIGNED_CONTEXT((#12784,#12786,#12787))
REPRESENTATION_CONTEXT('','3D')
);
#12764=(
GEOMETRIC_REPRESENTATION_CONTEXT(3)
GLOBAL_UNCERTAINTY_ASSIGNED_CONTEXT((#12720))
GLOBAL_UNIT_ASSIGNED_CONTEXT((#12784,#12786,#12787))
REPRESENTATION_CONTEXT('','3D')
);
#12765=(
GEOMETRIC_REPRESENTATION_CONTEXT(3)
GLOBAL_UNCERTAINTY_ASSIGNED_CONTEXT((#12721))
GLOBAL_UNIT_ASSIGNED_CONTEXT((#12784,#12786,#12787))
REPRESENTATION_CONTEXT('','3D')
);
#12766=(
GEOMETRIC_REPRESENTATION_CONTEXT(3)
GLOBAL_UNCERTAINTY_ASSIGNED_CONTEXT((#12722))
GLOBAL_UNIT_ASSIGNED_CONTEXT((#12784,#12786,#12787))
REPRESENTATION_CONTEXT('','3D')
);
#12767=(
GEOMETRIC_REPRESENTATION_CONTEXT(3)
GLOBAL_UNCERTAINTY_ASSIGNED_CONTEXT((#12723))
GLOBAL_UNIT_ASSIGNED_CONTEXT((#12784,#12786,#12787))
REPRESENTATION_CONTEXT('','3D')
);
#12768=(
GEOMETRIC_REPRESENTATION_CONTEXT(3)
GLOBAL_UNCERTAINTY_ASSIGNED_CONTEXT((#12724))
GLOBAL_UNIT_ASSIGNED_CONTEXT((#12784,#12786,#12787))
REPRESENTATION_CONTEXT('','3D')
);
#12769=(
GEOMETRIC_REPRESENTATION_CONTEXT(3)
GLOBAL_UNCERTAINTY_ASSIGNED_CONTEXT((#12725))
GLOBAL_UNIT_ASSIGNED_CONTEXT((#12784,#12786,#12787))
REPRESENTATION_CONTEXT('','3D')
);
#12770=(
GEOMETRIC_REPRESENTATION_CONTEXT(3)
GLOBAL_UNCERTAINTY_ASSIGNED_CONTEXT((#12726))
GLOBAL_UNIT_ASSIGNED_CONTEXT((#12784,#12786,#12787))
REPRESENTATION_CONTEXT('','3D')
);
#12771=(
GEOMETRIC_REPRESENTATION_CONTEXT(3)
GLOBAL_UNCERTAINTY_ASSIGNED_CONTEXT((#12727))
GLOBAL_UNIT_ASSIGNED_CONTEXT((#12784,#12786,#12787))
REPRESENTATION_CONTEXT('','3D')
);
#12772=(
GEOMETRIC_REPRESENTATION_CONTEXT(3)
GLOBAL_UNCERTAINTY_ASSIGNED_CONTEXT((#12728))
GLOBAL_UNIT_ASSIGNED_CONTEXT((#12784,#12786,#12787))
REPRESENTATION_CONTEXT('','3D')
);
#12773=(
GEOMETRIC_REPRESENTATION_CONTEXT(3)
GLOBAL_UNCERTAINTY_ASSIGNED_CONTEXT((#12729))
GLOBAL_UNIT_ASSIGNED_CONTEXT((#12784,#12786,#12787))
REPRESENTATION_CONTEXT('','3D')
);
#12774=(
GEOMETRIC_REPRESENTATION_CONTEXT(3)
GLOBAL_UNCERTAINTY_ASSIGNED_CONTEXT((#12730))
GLOBAL_UNIT_ASSIGNED_CONTEXT((#12784,#12786,#12787))
REPRESENTATION_CONTEXT('','3D')
);
#12775=(
GEOMETRIC_REPRESENTATION_CONTEXT(3)
GLOBAL_UNCERTAINTY_ASSIGNED_CONTEXT((#12731))
GLOBAL_UNIT_ASSIGNED_CONTEXT((#12784,#12786,#12787))
REPRESENTATION_CONTEXT('','3D')
);
#12776=(
GEOMETRIC_REPRESENTATION_CONTEXT(3)
GLOBAL_UNCERTAINTY_ASSIGNED_CONTEXT((#12732))
GLOBAL_UNIT_ASSIGNED_CONTEXT((#12784,#12786,#12787))
REPRESENTATION_CONTEXT('','3D')
);
#12777=(
GEOMETRIC_REPRESENTATION_CONTEXT(3)
GLOBAL_UNCERTAINTY_ASSIGNED_CONTEXT((#12733))
GLOBAL_UNIT_ASSIGNED_CONTEXT((#12784,#12786,#12787))
REPRESENTATION_CONTEXT('','3D')
);
#12778=(
GEOMETRIC_REPRESENTATION_CONTEXT(3)
GLOBAL_UNCERTAINTY_ASSIGNED_CONTEXT((#12734))
GLOBAL_UNIT_ASSIGNED_CONTEXT((#12784,#12786,#12787))
REPRESENTATION_CONTEXT('','3D')
);
#12779=(
GEOMETRIC_REPRESENTATION_CONTEXT(3)
GLOBAL_UNCERTAINTY_ASSIGNED_CONTEXT((#12735))
GLOBAL_UNIT_ASSIGNED_CONTEXT((#12784,#12786,#12787))
REPRESENTATION_CONTEXT('','3D')
);
#12780=(
GEOMETRIC_REPRESENTATION_CONTEXT(3)
GLOBAL_UNCERTAINTY_ASSIGNED_CONTEXT((#12736))
GLOBAL_UNIT_ASSIGNED_CONTEXT((#12784,#12786,#12787))
REPRESENTATION_CONTEXT('','3D')
);
#12781=(
GEOMETRIC_REPRESENTATION_CONTEXT(3)
GLOBAL_UNCERTAINTY_ASSIGNED_CONTEXT((#12737))
GLOBAL_UNIT_ASSIGNED_CONTEXT((#12784,#12786,#12787))
REPRESENTATION_CONTEXT('','3D')
);
#12782=(
GEOMETRIC_REPRESENTATION_CONTEXT(3)
GLOBAL_UNCERTAINTY_ASSIGNED_CONTEXT((#12738))
GLOBAL_UNIT_ASSIGNED_CONTEXT((#12784,#12786,#12787))
REPRESENTATION_CONTEXT('','3D')
);
#12783=(
GEOMETRIC_REPRESENTATION_CONTEXT(3)
GLOBAL_UNCERTAINTY_ASSIGNED_CONTEXT((#12739))
GLOBAL_UNIT_ASSIGNED_CONTEXT((#12784,#12786,#12787))
REPRESENTATION_CONTEXT('','3D')
);
#12784=(
LENGTH_UNIT()
NAMED_UNIT(*)
SI_UNIT(.CENTI.,.METRE.)
);
#12785=(
LENGTH_UNIT()
NAMED_UNIT(*)
SI_UNIT($,.METRE.)
);
#12786=(
NAMED_UNIT(*)
PLANE_ANGLE_UNIT()
SI_UNIT($,.RADIAN.)
);
#12787=(
NAMED_UNIT(*)
SI_UNIT($,.STERADIAN.)
SOLID_ANGLE_UNIT()
);
#12788=SHAPE_DEFINITION_REPRESENTATION(#12831,#12931);
#12789=SHAPE_DEFINITION_REPRESENTATION(#12832,#12932);
#12790=SHAPE_DEFINITION_REPRESENTATION(#12833,#12933);
#12791=SHAPE_DEFINITION_REPRESENTATION(#12834,#12934);
#12792=SHAPE_DEFINITION_REPRESENTATION(#12835,#12935);
#12793=SHAPE_DEFINITION_REPRESENTATION(#12836,#12936);
#12794=SHAPE_DEFINITION_REPRESENTATION(#12837,#12937);
#12795=SHAPE_DEFINITION_REPRESENTATION(#12838,#12938);
#12796=SHAPE_DEFINITION_REPRESENTATION(#12839,#12939);
#12797=SHAPE_DEFINITION_REPRESENTATION(#12840,#12940);
#12798=SHAPE_DEFINITION_REPRESENTATION(#12841,#12941);
#12799=SHAPE_DEFINITION_REPRESENTATION(#12842,#12942);
#12800=SHAPE_DEFINITION_REPRESENTATION(#12843,#12943);
#12801=SHAPE_DEFINITION_REPRESENTATION(#12844,#12944);
#12802=SHAPE_DEFINITION_REPRESENTATION(#12845,#12945);
#12803=SHAPE_DEFINITION_REPRESENTATION(#12851,#12946);
#12804=SHAPE_DEFINITION_REPRESENTATION(#12852,#12947);
#12805=SHAPE_DEFINITION_REPRESENTATION(#12874,#12948);
#12806=SHAPE_DEFINITION_REPRESENTATION(#12875,#12949);
#12807=SHAPE_DEFINITION_REPRESENTATION(#12876,#12950);
#12808=SHAPE_DEFINITION_REPRESENTATION(#12877,#12951);
#12809=SHAPE_DEFINITION_REPRESENTATION(#12878,#12952);
#12810=SHAPE_DEFINITION_REPRESENTATION(#12879,#12953);
#12811=SHAPE_DEFINITION_REPRESENTATION(#12880,#12954);
#12812=SHAPE_DEFINITION_REPRESENTATION(#12881,#12955);
#12813=SHAPE_DEFINITION_REPRESENTATION(#12882,#12956);
#12814=SHAPE_DEFINITION_REPRESENTATION(#12883,#12957);
#12815=SHAPE_DEFINITION_REPRESENTATION(#12884,#12958);
#12816=SHAPE_DEFINITION_REPRESENTATION(#12885,#12959);
#12817=SHAPE_DEFINITION_REPRESENTATION(#12886,#12960);
#12818=SHAPE_DEFINITION_REPRESENTATION(#12887,#12961);
#12819=SHAPE_DEFINITION_REPRESENTATION(#12888,#12962);
#12820=SHAPE_DEFINITION_REPRESENTATION(#12889,#12963);
#12821=SHAPE_DEFINITION_REPRESENTATION(#12908,#12964);
#12822=SHAPE_DEFINITION_REPRESENTATION(#12909,#12965);
#12823=SHAPE_DEFINITION_REPRESENTATION(#12910,#12966);
#12824=SHAPE_DEFINITION_REPRESENTATION(#12911,#12967);
#12825=SHAPE_DEFINITION_REPRESENTATION(#12912,#12968);
#12826=SHAPE_DEFINITION_REPRESENTATION(#12913,#12969);
#12827=SHAPE_DEFINITION_REPRESENTATION(#12914,#12970);
#12828=SHAPE_DEFINITION_REPRESENTATION(#12915,#12971);
#12829=SHAPE_DEFINITION_REPRESENTATION(#12916,#12972);
#12830=SHAPE_DEFINITION_REPRESENTATION(#12917,#12973);
#12831=PRODUCT_DEFINITION_SHAPE('',$,#12975);
#12832=PRODUCT_DEFINITION_SHAPE('',$,#12976);
#12833=PRODUCT_DEFINITION_SHAPE('',$,#12977);
#12834=PRODUCT_DEFINITION_SHAPE('',$,#12978);
#12835=PRODUCT_DEFINITION_SHAPE('',$,#12979);
#12836=PRODUCT_DEFINITION_SHAPE('',$,#12980);
#12837=PRODUCT_DEFINITION_SHAPE('',$,#12981);
#12838=PRODUCT_DEFINITION_SHAPE('',$,#12982);
#12839=PRODUCT_DEFINITION_SHAPE('',$,#12983);
#12840=PRODUCT_DEFINITION_SHAPE('',$,#12984);
#12841=PRODUCT_DEFINITION_SHAPE('',$,#12985);
#12842=PRODUCT_DEFINITION_SHAPE('',$,#12986);
#12843=PRODUCT_DEFINITION_SHAPE('',$,#12987);
#12844=PRODUCT_DEFINITION_SHAPE('',$,#12988);
#12845=PRODUCT_DEFINITION_SHAPE('',$,#12989);
#12846=PRODUCT_DEFINITION_SHAPE($,$,#188);
#12847=PRODUCT_DEFINITION_SHAPE($,$,#189);
#12848=PRODUCT_DEFINITION_SHAPE($,$,#190);
#12849=PRODUCT_DEFINITION_SHAPE($,$,#191);
#12850=PRODUCT_DEFINITION_SHAPE($,$,#192);
#12851=PRODUCT_DEFINITION_SHAPE('',$,#12990);
#12852=PRODUCT_DEFINITION_SHAPE('',$,#12991);
#12853=PRODUCT_DEFINITION_SHAPE($,$,#193);
#12854=PRODUCT_DEFINITION_SHAPE($,$,#194);
#12855=PRODUCT_DEFINITION_SHAPE($,$,#195);
#12856=PRODUCT_DEFINITION_SHAPE($,$,#196);
#12857=PRODUCT_DEFINITION_SHAPE($,$,#197);
#12858=PRODUCT_DEFINITION_SHAPE($,$,#198);
#12859=PRODUCT_DEFINITION_SHAPE($,$,#199);
#12860=PRODUCT_DEFINITION_SHAPE($,$,#200);
#12861=PRODUCT_DEFINITION_SHAPE($,$,#201);
#12862=PRODUCT_DEFINITION_SHAPE($,$,#202);
#12863=PRODUCT_DEFINITION_SHAPE($,$,#203);
#12864=PRODUCT_DEFINITION_SHAPE($,$,#204);
#12865=PRODUCT_DEFINITION_SHAPE($,$,#205);
#12866=PRODUCT_DEFINITION_SHAPE($,$,#206);
#12867=PRODUCT_DEFINITION_SHAPE($,$,#207);
#12868=PRODUCT_DEFINITION_SHAPE($,$,#208);
#12869=PRODUCT_DEFINITION_SHAPE($,$,#209);
#12870=PRODUCT_DEFINITION_SHAPE($,$,#210);
#12871=PRODUCT_DEFINITION_SHAPE($,$,#211);
#12872=PRODUCT_DEFINITION_SHAPE($,$,#212);
#12873=PRODUCT_DEFINITION_SHAPE($,$,#213);
#12874=PRODUCT_DEFINITION_SHAPE('',$,#12992);
#12875=PRODUCT_DEFINITION_SHAPE('',$,#12993);
#12876=PRODUCT_DEFINITION_SHAPE('',$,#12994);
#12877=PRODUCT_DEFINITION_SHAPE('',$,#12995);
#12878=PRODUCT_DEFINITION_SHAPE('',$,#12996);
#12879=PRODUCT_DEFINITION_SHAPE('',$,#12997);
#12880=PRODUCT_DEFINITION_SHAPE('',$,#12998);
#12881=PRODUCT_DEFINITION_SHAPE('',$,#12999);
#12882=PRODUCT_DEFINITION_SHAPE('',$,#13000);
#12883=PRODUCT_DEFINITION_SHAPE('',$,#13001);
#12884=PRODUCT_DEFINITION_SHAPE('',$,#13002);
#12885=PRODUCT_DEFINITION_SHAPE('',$,#13003);
#12886=PRODUCT_DEFINITION_SHAPE('',$,#13004);
#12887=PRODUCT_DEFINITION_SHAPE('',$,#13005);
#12888=PRODUCT_DEFINITION_SHAPE('',$,#13006);
#12889=PRODUCT_DEFINITION_SHAPE('',$,#13007);
#12890=PRODUCT_DEFINITION_SHAPE($,$,#214);
#12891=PRODUCT_DEFINITION_SHAPE($,$,#215);
#12892=PRODUCT_DEFINITION_SHAPE($,$,#216);
#12893=PRODUCT_DEFINITION_SHAPE($,$,#217);
#12894=PRODUCT_DEFINITION_SHAPE($,$,#218);
#12895=PRODUCT_DEFINITION_SHAPE($,$,#219);
#12896=PRODUCT_DEFINITION_SHAPE($,$,#220);
#12897=PRODUCT_DEFINITION_SHAPE($,$,#221);
#12898=PRODUCT_DEFINITION_SHAPE($,$,#222);
#12899=PRODUCT_DEFINITION_SHAPE($,$,#223);
#12900=PRODUCT_DEFINITION_SHAPE($,$,#224);
#12901=PRODUCT_DEFINITION_SHAPE($,$,#225);
#12902=PRODUCT_DEFINITION_SHAPE($,$,#226);
#12903=PRODUCT_DEFINITION_SHAPE($,$,#227);
#12904=PRODUCT_DEFINITION_SHAPE($,$,#228);
#12905=PRODUCT_DEFINITION_SHAPE($,$,#229);
#12906=PRODUCT_DEFINITION_SHAPE($,$,#230);
#12907=PRODUCT_DEFINITION_SHAPE($,$,#231);
#12908=PRODUCT_DEFINITION_SHAPE('',$,#13008);
#12909=PRODUCT_DEFINITION_SHAPE('',$,#13009);
#12910=PRODUCT_DEFINITION_SHAPE('',$,#13010);
#12911=PRODUCT_DEFINITION_SHAPE('',$,#13011);
#12912=PRODUCT_DEFINITION_SHAPE('',$,#13012);
#12913=PRODUCT_DEFINITION_SHAPE('',$,#13013);
#12914=PRODUCT_DEFINITION_SHAPE('',$,#13014);
#12915=PRODUCT_DEFINITION_SHAPE('',$,#13015);
#12916=PRODUCT_DEFINITION_SHAPE('',$,#13016);
#12917=PRODUCT_DEFINITION_SHAPE('',$,#13017);
#12918=PRODUCT_DEFINITION_SHAPE($,$,#232);
#12919=PRODUCT_DEFINITION_SHAPE($,$,#233);
#12920=PRODUCT_DEFINITION_SHAPE($,$,#234);
#12921=PRODUCT_DEFINITION_SHAPE($,$,#235);
#12922=PRODUCT_DEFINITION_SHAPE($,$,#236);
#12923=PRODUCT_DEFINITION_SHAPE($,$,#237);
#12924=PRODUCT_DEFINITION_SHAPE($,$,#238);
#12925=PRODUCT_DEFINITION_SHAPE($,$,#239);
#12926=PRODUCT_DEFINITION_SHAPE($,$,#240);
#12927=PRODUCT_DEFINITION_SHAPE($,$,#241);
#12928=PRODUCT_DEFINITION_SHAPE($,$,#242);
#12929=PRODUCT_DEFINITION_SHAPE($,$,#243);
#12930=PRODUCT_DEFINITION_SHAPE($,$,#244);
#12931=SHAPE_REPRESENTATION('',(#6960,#7807,#7808,#7809),#12740);
#12932=SHAPE_REPRESENTATION('',(#6961,#7353,#7354,#7355,#7356,#7357,#7358,
#7359,#7360,#7361,#7362,#7363,#7364,#7365,#7366,#7367,#7368,#7369,#7370,
#7371,#7372,#7373),#12741);
#12933=SHAPE_REPRESENTATION('',(#6962),#12742);
#12934=SHAPE_REPRESENTATION('',(#6981),#12743);
#12935=SHAPE_REPRESENTATION('',(#7084),#12744);
#12936=SHAPE_REPRESENTATION('',(#7093),#12745);
#12937=SHAPE_REPRESENTATION('',(#7118),#12746);
#12938=SHAPE_REPRESENTATION('',(#7143),#12747);
#12939=SHAPE_REPRESENTATION('',(#7150),#12748);
#12940=SHAPE_REPRESENTATION('',(#7157,#7296,#7297,#7298,#7299,#7300),#12749);
#12941=SHAPE_REPRESENTATION('',(#7158),#12750);
#12942=SHAPE_REPRESENTATION('',(#7178),#12751);
#12943=SHAPE_REPRESENTATION('',(#7198),#12752);
#12944=SHAPE_REPRESENTATION('',(#7217),#12753);
#12945=SHAPE_REPRESENTATION('',(#7279),#12754);
#12946=SHAPE_REPRESENTATION('',(#7301),#12755);
#12947=SHAPE_REPRESENTATION('',(#7327),#12756);
#12948=SHAPE_REPRESENTATION('',(#7374,#7671,#7672,#7673,#7674,#7675,#7676,
#7677,#7678,#7679,#7680,#7681,#7682,#7683),#12757);
#12949=SHAPE_REPRESENTATION('',(#7375),#12758);
#12950=SHAPE_REPRESENTATION('',(#7403),#12759);
#12951=SHAPE_REPRESENTATION('',(#7412),#12760);
#12952=SHAPE_REPRESENTATION('',(#7427),#12761);
#12953=SHAPE_REPRESENTATION('',(#7453),#12762);
#12954=SHAPE_REPRESENTATION('',(#7483),#12763);
#12955=SHAPE_REPRESENTATION('',(#7496),#12764);
#12956=SHAPE_REPRESENTATION('',(#7509),#12765);
#12957=SHAPE_REPRESENTATION('',(#7520),#12766);
#12958=SHAPE_REPRESENTATION('',(#7537,#7666,#7667,#7668,#7669,#7670),#12767);
#12959=SHAPE_REPRESENTATION('',(#7538),#12768);
#12960=SHAPE_REPRESENTATION('',(#7558),#12769);
#12961=SHAPE_REPRESENTATION('',(#7578),#12770);
#12962=SHAPE_REPRESENTATION('',(#7595),#12771);
#12963=SHAPE_REPRESENTATION('',(#7649),#12772);
#12964=SHAPE_REPRESENTATION('',(#7684,#7797,#7798,#7799,#7800,#7801,#7802,
#7803,#7804,#7805,#7806),#12773);
#12965=SHAPE_REPRESENTATION('',(#7685),#12774);
#12966=SHAPE_REPRESENTATION('',(#7705),#12775);
#12967=SHAPE_REPRESENTATION('',(#7719),#12776);
#12968=SHAPE_REPRESENTATION('',(#7728),#12777);
#12969=SHAPE_REPRESENTATION('',(#7737),#12778);
#12970=SHAPE_REPRESENTATION('',(#7746),#12779);
#12971=SHAPE_REPRESENTATION('',(#7755),#12780);
#12972=SHAPE_REPRESENTATION('',(#7764),#12781);
#12973=SHAPE_REPRESENTATION('',(#7773),#12782);
#12974=PRODUCT_DEFINITION_CONTEXT('part definition',#13105,'design');
#12975=PRODUCT_DEFINITION('PAT-105','PAT-105',#13018,
#12974);
#12976=PRODUCT_DEFINITION('Bearing stand','Bearing stand',#13019,#12974);
#12977=PRODUCT_DEFINITION('Base','Base',#13020,#12974);
#12978=PRODUCT_DEFINITION('Bearing housing','Bearing housing',#13021,#12974);
#12979=PRODUCT_DEFINITION('Outer race spacer','Outer race spacer',#13022,
#12974);
#12980=PRODUCT_DEFINITION('Bearing cap','Bearing cap',#13023,#12974);
#12981=PRODUCT_DEFINITION('Bearing cap (1)','Bearing cap (1)',#13024,#12974);
#12982=PRODUCT_DEFINITION('Bonded foot','Bonded foot',#13025,#12974);
#12983=PRODUCT_DEFINITION('Bonded foot (1)','Bonded foot (1)',#13026,#12974);
#12984=PRODUCT_DEFINITION('Sealed Ball Bearing - 25 x 52 x 15 mm',
'Sealed Ball Bearing - 25 x 52 x 15 mm',#13027,#12974);
#12985=PRODUCT_DEFINITION('Inner ring','Inner ring',#13028,#12974);
#12986=PRODUCT_DEFINITION('Outer ring','Outer ring',#13029,#12974);
#12987=PRODUCT_DEFINITION('Balls','Balls',#13030,#12974);
#12988=PRODUCT_DEFINITION('Cage','Cage',#13031,#12974);
#12989=PRODUCT_DEFINITION('Seals 2RS','Seals 2RS',#13032,#12974);
#12990=PRODUCT_DEFINITION('Cap Screw - M6x25','Cap Screw - M6x25',#13033,
#12974);
#12991=PRODUCT_DEFINITION('Cap Screw - M4x16','Cap Screw - M4x16',#13034,
#12974);
#12992=PRODUCT_DEFINITION('Shaft and torque arm','Shaft and torque arm',
#13035,#12974);
#12993=PRODUCT_DEFINITION('Shaft','Shaft',#13036,#12974);
#12994=PRODUCT_DEFINITION('Inner race spacer','Inner race spacer',#13037,
#12974);
#12995=PRODUCT_DEFINITION('Shaft collar','Shaft collar',#13038,#12974);
#12996=PRODUCT_DEFINITION('Square drive adapter','Square drive adapter',
#13039,#12974);
#12997=PRODUCT_DEFINITION('Torque arm','Torque arm',#13040,#12974);
#12998=PRODUCT_DEFINITION('Hanger bearing retainer',
'Hanger bearing retainer',#13041,#12974);
#12999=PRODUCT_DEFINITION('Hanger bearing retainer (1)',
'Hanger bearing retainer (1)',#13042,#12974);
#13000=PRODUCT_DEFINITION('Key 8x7x20','Key 8x7x20',#13043,#12974);
#13001=PRODUCT_DEFINITION('Socket Set Screw - M5x8',
'Socket Set Screw - M5x8',#13044,#12974);
#13002=PRODUCT_DEFINITION('Sealed Ball Bearing - 10 x 30 x 9 mm',
'Sealed Ball Bearing - 10 x 30 x 9 mm',#13045,#12974);
#13003=PRODUCT_DEFINITION('Inner ring (1)','Inner ring (1)',#13046,#12974);
#13004=PRODUCT_DEFINITION('Outer ring (1)','Outer ring (1)',#13047,#12974);
#13005=PRODUCT_DEFINITION('Balls (1)','Balls (1)',#13048,#12974);
#13006=PRODUCT_DEFINITION('Cage (1)','Cage (1)',#13049,#12974);
#13007=PRODUCT_DEFINITION('Seals 2RS (1)','Seals 2RS (1)',#13050,#12974);
#13008=PRODUCT_DEFINITION('Weight hanger (1)','Weight hanger (1)',#13051,#12974);
#13009=PRODUCT_DEFINITION('Weight hanger','Weight hanger',#13052,#12974);
#13010=PRODUCT_DEFINITION('Hanger axle','Hanger axle',#13053,#12974);
#13011=PRODUCT_DEFINITION('Hanger inner spacer','Hanger inner spacer',#13054,
#12974);
#13012=PRODUCT_DEFINITION('Hanger inner spacer (1)',
'Hanger inner spacer (1)',#13055,#12974);
#13013=PRODUCT_DEFINITION('Hanger outer shim','Hanger outer shim',#13056,
#12974);
#13014=PRODUCT_DEFINITION('Hanger outer shim (1)','Hanger outer shim (1)',
#13057,#12974);
#13015=PRODUCT_DEFINITION('Hanger keeper','Hanger keeper',#13058,#12974);
#13016=PRODUCT_DEFINITION('Hanger keeper (1)','Hanger keeper (1)',#13059,
#12974);
#13017=PRODUCT_DEFINITION('M4x10 Cap Screw','M4x10 Cap Screw',#13060,#12974);
#13018=PRODUCT_DEFINITION_FORMATION('',$,#13107);
#13019=PRODUCT_DEFINITION_FORMATION('',$,#13108);
#13020=PRODUCT_DEFINITION_FORMATION('',$,#13109);
#13021=PRODUCT_DEFINITION_FORMATION('',$,#13110);
#13022=PRODUCT_DEFINITION_FORMATION('',$,#13111);
#13023=PRODUCT_DEFINITION_FORMATION('',$,#13112);
#13024=PRODUCT_DEFINITION_FORMATION('',$,#13113);
#13025=PRODUCT_DEFINITION_FORMATION('',$,#13114);
#13026=PRODUCT_DEFINITION_FORMATION('',$,#13115);
#13027=PRODUCT_DEFINITION_FORMATION('',$,#13116);
#13028=PRODUCT_DEFINITION_FORMATION('',$,#13117);
#13029=PRODUCT_DEFINITION_FORMATION('',$,#13118);
#13030=PRODUCT_DEFINITION_FORMATION('',$,#13119);
#13031=PRODUCT_DEFINITION_FORMATION('',$,#13120);
#13032=PRODUCT_DEFINITION_FORMATION('',$,#13121);
#13033=PRODUCT_DEFINITION_FORMATION('',$,#13122);
#13034=PRODUCT_DEFINITION_FORMATION('',$,#13123);
#13035=PRODUCT_DEFINITION_FORMATION('',$,#13124);
#13036=PRODUCT_DEFINITION_FORMATION('',$,#13125);
#13037=PRODUCT_DEFINITION_FORMATION('',$,#13126);
#13038=PRODUCT_DEFINITION_FORMATION('',$,#13127);
#13039=PRODUCT_DEFINITION_FORMATION('',$,#13128);
#13040=PRODUCT_DEFINITION_FORMATION('',$,#13129);
#13041=PRODUCT_DEFINITION_FORMATION('',$,#13130);
#13042=PRODUCT_DEFINITION_FORMATION('',$,#13131);
#13043=PRODUCT_DEFINITION_FORMATION('',$,#13132);
#13044=PRODUCT_DEFINITION_FORMATION('',$,#13133);
#13045=PRODUCT_DEFINITION_FORMATION('',$,#13134);
#13046=PRODUCT_DEFINITION_FORMATION('',$,#13135);
#13047=PRODUCT_DEFINITION_FORMATION('',$,#13136);
#13048=PRODUCT_DEFINITION_FORMATION('',$,#13137);
#13049=PRODUCT_DEFINITION_FORMATION('',$,#13138);
#13050=PRODUCT_DEFINITION_FORMATION('',$,#13139);
#13051=PRODUCT_DEFINITION_FORMATION('',$,#13140);
#13052=PRODUCT_DEFINITION_FORMATION('',$,#13141);
#13053=PRODUCT_DEFINITION_FORMATION('',$,#13142);
#13054=PRODUCT_DEFINITION_FORMATION('',$,#13143);
#13055=PRODUCT_DEFINITION_FORMATION('',$,#13144);
#13056=PRODUCT_DEFINITION_FORMATION('',$,#13145);
#13057=PRODUCT_DEFINITION_FORMATION('',$,#13146);
#13058=PRODUCT_DEFINITION_FORMATION('',$,#13147);
#13059=PRODUCT_DEFINITION_FORMATION('',$,#13148);
#13060=PRODUCT_DEFINITION_FORMATION('',$,#13149);
#13061=PRODUCT_RELATED_PRODUCT_CATEGORY('PAT-105','PAT-105',(#13107));
#13062=PRODUCT_RELATED_PRODUCT_CATEGORY('Bearing stand','Bearing stand',
(#13108));
#13063=PRODUCT_RELATED_PRODUCT_CATEGORY('Base','Base',(#13109));
#13064=PRODUCT_RELATED_PRODUCT_CATEGORY('Bearing housing',
'Bearing housing',(#13110));
#13065=PRODUCT_RELATED_PRODUCT_CATEGORY('Outer race spacer',
'Outer race spacer',(#13111));
#13066=PRODUCT_RELATED_PRODUCT_CATEGORY('Bearing cap','Bearing cap',(#13112));
#13067=PRODUCT_RELATED_PRODUCT_CATEGORY('Bearing cap (1)',
'Bearing cap (1)',(#13113));
#13068=PRODUCT_RELATED_PRODUCT_CATEGORY('Bonded foot','Bonded foot',(#13114));
#13069=PRODUCT_RELATED_PRODUCT_CATEGORY('Bonded foot (1)',
'Bonded foot (1)',(#13115));
#13070=PRODUCT_RELATED_PRODUCT_CATEGORY(
'Sealed Ball Bearing - 25 x 52 x 15 mm',
'Sealed Ball Bearing - 25 x 52 x 15 mm',(#13116));
#13071=PRODUCT_RELATED_PRODUCT_CATEGORY('Inner ring','Inner ring',(#13117));
#13072=PRODUCT_RELATED_PRODUCT_CATEGORY('Outer ring','Outer ring',(#13118));
#13073=PRODUCT_RELATED_PRODUCT_CATEGORY('Balls','Balls',(#13119));
#13074=PRODUCT_RELATED_PRODUCT_CATEGORY('Cage','Cage',(#13120));
#13075=PRODUCT_RELATED_PRODUCT_CATEGORY('Seals 2RS','Seals 2RS',(#13121));
#13076=PRODUCT_RELATED_PRODUCT_CATEGORY('Cap Screw - M6x25',
'Cap Screw - M6x25',(#13122));
#13077=PRODUCT_RELATED_PRODUCT_CATEGORY('Cap Screw - M4x16',
'Cap Screw - M4x16',(#13123));
#13078=PRODUCT_RELATED_PRODUCT_CATEGORY('Shaft and torque arm',
'Shaft and torque arm',(#13124));
#13079=PRODUCT_RELATED_PRODUCT_CATEGORY('Shaft','Shaft',(#13125));
#13080=PRODUCT_RELATED_PRODUCT_CATEGORY('Inner race spacer',
'Inner race spacer',(#13126));
#13081=PRODUCT_RELATED_PRODUCT_CATEGORY('Shaft collar','Shaft collar',(#13127));
#13082=PRODUCT_RELATED_PRODUCT_CATEGORY('Square drive adapter',
'Square drive adapter',(#13128));
#13083=PRODUCT_RELATED_PRODUCT_CATEGORY('Torque arm','Torque arm',(#13129));
#13084=PRODUCT_RELATED_PRODUCT_CATEGORY('Hanger bearing retainer',
'Hanger bearing retainer',(#13130));
#13085=PRODUCT_RELATED_PRODUCT_CATEGORY('Hanger bearing retainer (1)',
'Hanger bearing retainer (1)',(#13131));
#13086=PRODUCT_RELATED_PRODUCT_CATEGORY('Key 8x7x20','Key 8x7x20',(#13132));
#13087=PRODUCT_RELATED_PRODUCT_CATEGORY('Socket Set Screw - M5x8',
'Socket Set Screw - M5x8',(#13133));
#13088=PRODUCT_RELATED_PRODUCT_CATEGORY(
'Sealed Ball Bearing - 10 x 30 x 9 mm',
'Sealed Ball Bearing - 10 x 30 x 9 mm',(#13134));
#13089=PRODUCT_RELATED_PRODUCT_CATEGORY('Inner ring (1)',
'Inner ring (1)',(#13135));
#13090=PRODUCT_RELATED_PRODUCT_CATEGORY('Outer ring (1)',
'Outer ring (1)',(#13136));
#13091=PRODUCT_RELATED_PRODUCT_CATEGORY('Balls (1)','Balls (1)',(#13137));
#13092=PRODUCT_RELATED_PRODUCT_CATEGORY('Cage (1)','Cage (1)',(#13138));
#13093=PRODUCT_RELATED_PRODUCT_CATEGORY('Seals 2RS (1)','Seals 2RS (1)',
(#13139));
#13094=PRODUCT_RELATED_PRODUCT_CATEGORY('Weight hanger (1)',
'Weight hanger (1)',(#13140));
#13095=PRODUCT_RELATED_PRODUCT_CATEGORY('Weight hanger','Weight hanger',
(#13141));
#13096=PRODUCT_RELATED_PRODUCT_CATEGORY('Hanger axle','Hanger axle',(#13142));
#13097=PRODUCT_RELATED_PRODUCT_CATEGORY('Hanger inner spacer',
'Hanger inner spacer',(#13143));
#13098=PRODUCT_RELATED_PRODUCT_CATEGORY('Hanger inner spacer (1)',
'Hanger inner spacer (1)',(#13144));
#13099=PRODUCT_RELATED_PRODUCT_CATEGORY('Hanger outer shim',
'Hanger outer shim',(#13145));
#13100=PRODUCT_RELATED_PRODUCT_CATEGORY('Hanger outer shim (1)',
'Hanger outer shim (1)',(#13146));
#13101=PRODUCT_RELATED_PRODUCT_CATEGORY('Hanger keeper','Hanger keeper',
(#13147));
#13102=PRODUCT_RELATED_PRODUCT_CATEGORY('Hanger keeper (1)',
'Hanger keeper (1)',(#13148));
#13103=PRODUCT_RELATED_PRODUCT_CATEGORY('M4x10 Cap Screw',
'M4x10 Cap Screw',(#13149));
#13104=APPLICATION_PROTOCOL_DEFINITION('international standard',
'automotive_design',2009,#13105);
#13105=APPLICATION_CONTEXT(
'Core Data for Automotive Mechanical Design Process');
#13106=PRODUCT_CONTEXT('part definition',#13105,'mechanical');
#13107=PRODUCT('PAT-105','PAT-105',
'PAT-105',(#13106));
#13108=PRODUCT('Bearing stand','Bearing stand','Bearing stand',(#13106));
#13109=PRODUCT('Base','Base','Base',(#13106));
#13110=PRODUCT('Bearing housing','Bearing housing','Bearing housing',(#13106));
#13111=PRODUCT('Outer race spacer','Outer race spacer',
'Outer race spacer',(#13106));
#13112=PRODUCT('Bearing cap','Bearing cap','Bearing cap',(#13106));
#13113=PRODUCT('Bearing cap (1)','Bearing cap (1)','Bearing cap (1)',(#13106));
#13114=PRODUCT('Bonded foot','Bonded foot','Bonded foot',(#13106));
#13115=PRODUCT('Bonded foot (1)','Bonded foot (1)','Bonded foot (1)',(#13106));
#13116=PRODUCT('Sealed Ball Bearing - 25 x 52 x 15 mm',
'Sealed Ball Bearing - 25 x 52 x 15 mm',
'Sealed Ball Bearing - 25 x 52 x 15 mm',(#13106));
#13117=PRODUCT('Inner ring','Inner ring','Inner ring',(#13106));
#13118=PRODUCT('Outer ring','Outer ring','Outer ring',(#13106));
#13119=PRODUCT('Balls','Balls','Balls',(#13106));
#13120=PRODUCT('Cage','Cage','Cage',(#13106));
#13121=PRODUCT('Seals 2RS','Seals 2RS','Seals 2RS',(#13106));
#13122=PRODUCT('Cap Screw - M6x25','Cap Screw - M6x25',
'Cap Screw - M6x25',(#13106));
#13123=PRODUCT('Cap Screw - M4x16','Cap Screw - M4x16',
'Cap Screw - M4x16',(#13106));
#13124=PRODUCT('Shaft and torque arm','Shaft and torque arm',
'Shaft and torque arm',(#13106));
#13125=PRODUCT('Shaft','Shaft','Shaft',(#13106));
#13126=PRODUCT('Inner race spacer','Inner race spacer',
'Inner race spacer',(#13106));
#13127=PRODUCT('Shaft collar','Shaft collar','Shaft collar',(#13106));
#13128=PRODUCT('Square drive adapter','Square drive adapter',
'Square drive adapter',(#13106));
#13129=PRODUCT('Torque arm','Torque arm','Torque arm',(#13106));
#13130=PRODUCT('Hanger bearing retainer','Hanger bearing retainer',
'Hanger bearing retainer',(#13106));
#13131=PRODUCT('Hanger bearing retainer (1)',
'Hanger bearing retainer (1)','Hanger bearing retainer (1)',(#13106));
#13132=PRODUCT('Key 8x7x20','Key 8x7x20','Key 8x7x20',(#13106));
#13133=PRODUCT('Socket Set Screw - M5x8','Socket Set Screw - M5x8',
'Socket Set Screw - M5x8',(#13106));
#13134=PRODUCT('Sealed Ball Bearing - 10 x 30 x 9 mm',
'Sealed Ball Bearing - 10 x 30 x 9 mm',
'Sealed Ball Bearing - 10 x 30 x 9 mm',(#13106));
#13135=PRODUCT('Inner ring (1)','Inner ring (1)','Inner ring (1)',(#13106));
#13136=PRODUCT('Outer ring (1)','Outer ring (1)','Outer ring (1)',(#13106));
#13137=PRODUCT('Balls (1)','Balls (1)','Balls (1)',(#13106));
#13138=PRODUCT('Cage (1)','Cage (1)','Cage (1)',(#13106));
#13139=PRODUCT('Seals 2RS (1)','Seals 2RS (1)','Seals 2RS (1)',(#13106));
#13140=PRODUCT('Weight hanger (1)','Weight hanger (1)','Weight hanger (1)',(#13106));
#13141=PRODUCT('Weight hanger','Weight hanger','Weight hanger',(#13106));
#13142=PRODUCT('Hanger axle','Hanger axle','Hanger axle',(#13106));
#13143=PRODUCT('Hanger inner spacer','Hanger inner spacer',
'Hanger inner spacer',(#13106));
#13144=PRODUCT('Hanger inner spacer (1)','Hanger inner spacer (1)',
'Hanger inner spacer (1)',(#13106));
#13145=PRODUCT('Hanger outer shim','Hanger outer shim',
'Hanger outer shim',(#13106));
#13146=PRODUCT('Hanger outer shim (1)','Hanger outer shim (1)',
'Hanger outer shim (1)',(#13106));
#13147=PRODUCT('Hanger keeper','Hanger keeper','Hanger keeper',(#13106));
#13148=PRODUCT('Hanger keeper (1)','Hanger keeper (1)','Hanger keeper (1)',(#13106));
#13149=PRODUCT('M4x10 Cap Screw','M4x10 Cap Screw','M4x10 Cap Screw',(#13106));
#13150=PRESENTATION_STYLE_ASSIGNMENT((#13155));
#13151=PRESENTATION_STYLE_ASSIGNMENT((#13156));
#13152=PRESENTATION_STYLE_ASSIGNMENT((#13157));
#13153=PRESENTATION_STYLE_ASSIGNMENT((#13158));
#13154=PRESENTATION_STYLE_ASSIGNMENT((#13159));
#13155=SURFACE_STYLE_USAGE(.BOTH.,#13160);
#13156=SURFACE_STYLE_USAGE(.BOTH.,#13161);
#13157=SURFACE_STYLE_USAGE(.BOTH.,#13162);
#13158=SURFACE_STYLE_USAGE(.BOTH.,#13163);
#13159=SURFACE_STYLE_USAGE(.BOTH.,#13164);
#13160=SURFACE_SIDE_STYLE('',(#13165));
#13161=SURFACE_SIDE_STYLE('',(#13166));
#13162=SURFACE_SIDE_STYLE('',(#13167));
#13163=SURFACE_SIDE_STYLE('',(#13168));
#13164=SURFACE_SIDE_STYLE('',(#13169));
#13165=SURFACE_STYLE_FILL_AREA(#13170);
#13166=SURFACE_STYLE_FILL_AREA(#13171);
#13167=SURFACE_STYLE_FILL_AREA(#13172);
#13168=SURFACE_STYLE_FILL_AREA(#13173);
#13169=SURFACE_STYLE_FILL_AREA(#13174);
#13170=FILL_AREA_STYLE('Steel - Satin',(#13175));
#13171=FILL_AREA_STYLE('CAD Library Painted - Deep blue',(#13176));
#13172=FILL_AREA_STYLE('CAD Library Painted - Steel gray',(#13177));
#13173=FILL_AREA_STYLE('CAD Library Painted - Engineering blue',(#13178));
#13174=FILL_AREA_STYLE('CAD Library Painted - Graphite',(#13179));
#13175=FILL_AREA_STYLE_COLOUR('Steel - Satin',#13180);
#13176=FILL_AREA_STYLE_COLOUR('CAD Library Painted - Deep blue',#13181);
#13177=FILL_AREA_STYLE_COLOUR('CAD Library Painted - Steel gray',#13182);
#13178=FILL_AREA_STYLE_COLOUR('CAD Library Painted - Engineering blue',
#13183);
#13179=FILL_AREA_STYLE_COLOUR('CAD Library Painted - Graphite',#13184);
#13180=COLOUR_RGB('Steel - Satin',0.627450980392157,0.627450980392157,0.627450980392157);
#13181=COLOUR_RGB('CAD Library Painted - Deep blue',0.0784313725490196,
0.203921568627451,0.349019607843137);
#13182=COLOUR_RGB('CAD Library Painted - Steel gray',0.592156862745098,
0.631372549019608,0.67843137254902);
#13183=COLOUR_RGB('CAD Library Painted - Engineering blue',0.12156862745098,
0.356862745098039,0.6);
#13184=COLOUR_RGB('CAD Library Painted - Graphite',0.168627450980392,0.192156862745098,
0.231372549019608);
#13185=COLOUR_RGB('Dark Blue',0.08,0.2,0.34);
#13186=FILL_AREA_STYLE_COLOUR('',#13185);
#13187=FILL_AREA_STYLE('',(#13186));
#13188=SURFACE_STYLE_FILL_AREA(#13187);
#13189=SURFACE_SIDE_STYLE('',(#13188));
#13190=SURFACE_STYLE_USAGE(.BOTH.,#13189);
#13191=PRESENTATION_STYLE_ASSIGNMENT((#13190));
#13192=COLOUR_RGB('Light Blue',0.38,0.62,0.78);
#13193=FILL_AREA_STYLE_COLOUR('',#13192);
#13194=FILL_AREA_STYLE('',(#13193));
#13195=SURFACE_STYLE_FILL_AREA(#13194);
#13196=SURFACE_SIDE_STYLE('',(#13195));
#13197=SURFACE_STYLE_USAGE(.BOTH.,#13196);
#13198=PRESENTATION_STYLE_ASSIGNMENT((#13197));
#13199=COLOUR_RGB('Sky Blue',0.24,0.69,0.87);
#13200=FILL_AREA_STYLE_COLOUR('',#13199);
#13201=FILL_AREA_STYLE('',(#13200));
#13202=SURFACE_STYLE_FILL_AREA(#13201);
#13203=SURFACE_SIDE_STYLE('',(#13202));
#13204=SURFACE_STYLE_USAGE(.BOTH.,#13203);
#13205=PRESENTATION_STYLE_ASSIGNMENT((#13204));
#13206=COLOUR_RGB('Grey',0.48,0.52,0.57);
#13207=FILL_AREA_STYLE_COLOUR('',#13206);
#13208=FILL_AREA_STYLE('',(#13207));
#13209=SURFACE_STYLE_FILL_AREA(#13208);
#13210=SURFACE_SIDE_STYLE('',(#13209));
#13211=SURFACE_STYLE_USAGE(.BOTH.,#13210);
#13212=PRESENTATION_STYLE_ASSIGNMENT((#13211));
#13213=COLOUR_RGB('Black',0.12,0.14,0.17);
#13214=FILL_AREA_STYLE_COLOUR('',#13213);
#13215=FILL_AREA_STYLE('',(#13214));
#13216=SURFACE_STYLE_FILL_AREA(#13215);
#13217=SURFACE_SIDE_STYLE('',(#13216));
#13218=SURFACE_STYLE_USAGE(.BOTH.,#13217);
#13219=PRESENTATION_STYLE_ASSIGNMENT((#13218));
#13220=COLOUR_RGB('Off White',0.89,0.88,0.83);
#13221=FILL_AREA_STYLE_COLOUR('',#13220);
#13222=FILL_AREA_STYLE('',(#13221));
#13223=SURFACE_STYLE_FILL_AREA(#13222);
#13224=SURFACE_SIDE_STYLE('',(#13223));
#13225=SURFACE_STYLE_USAGE(.BOTH.,#13224);
#13226=PRESENTATION_STYLE_ASSIGNMENT((#13225));
ENDSEC;
END-ISO-10303-21;
